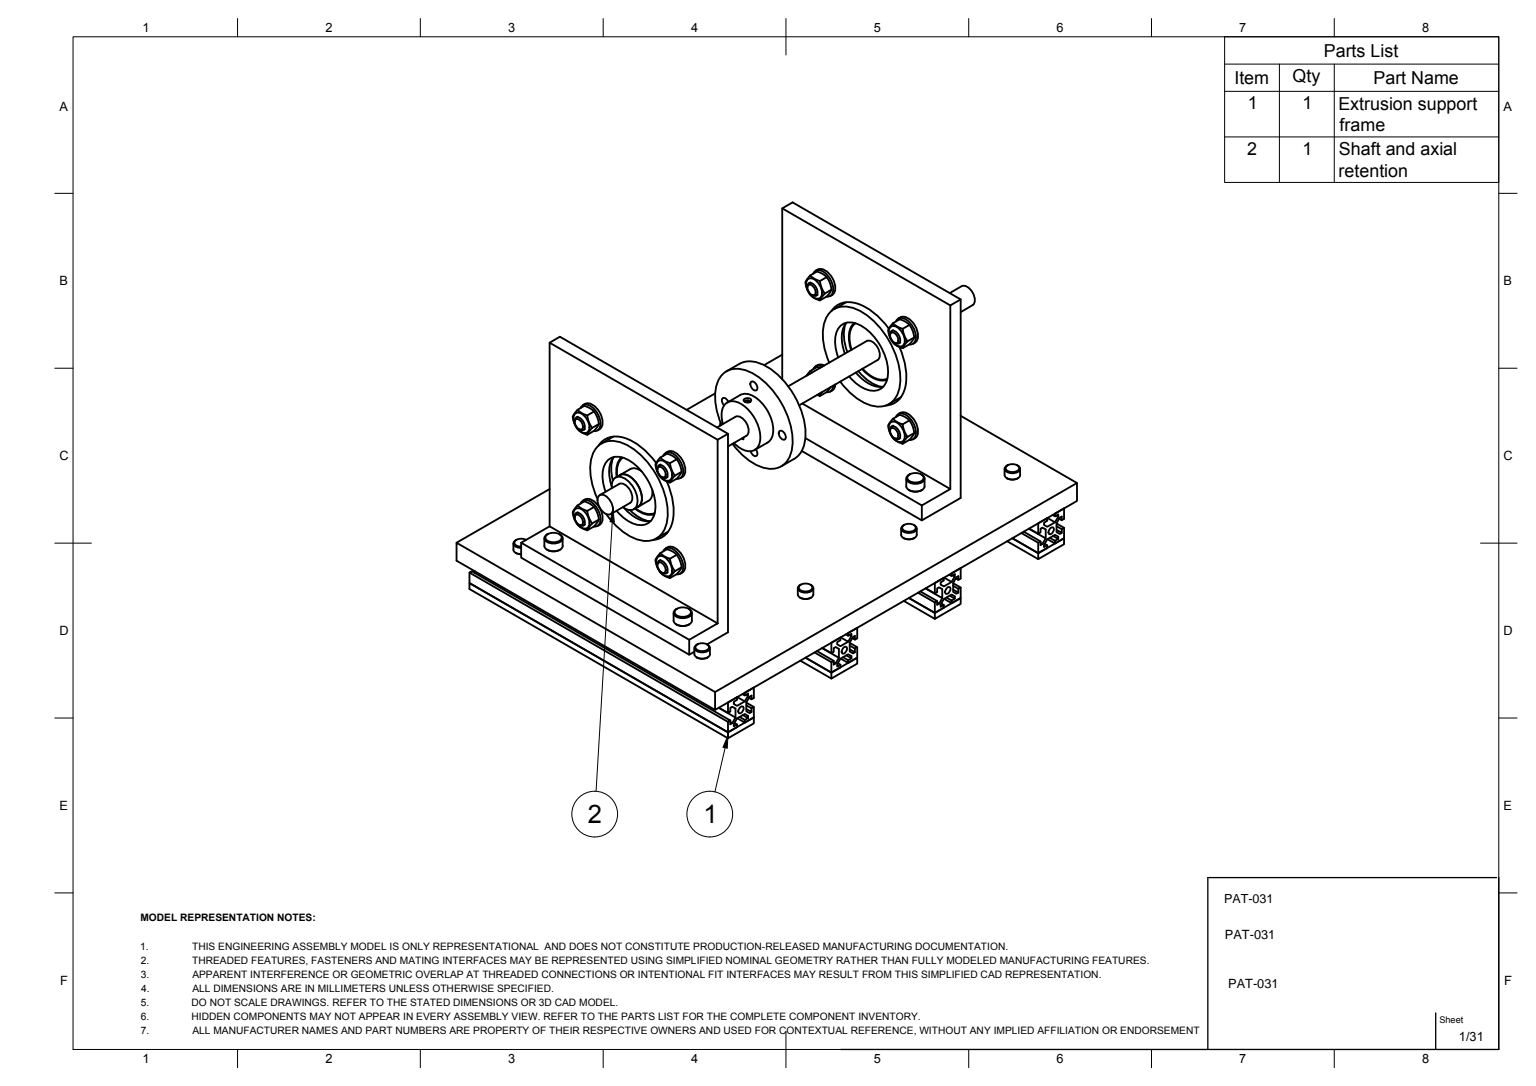
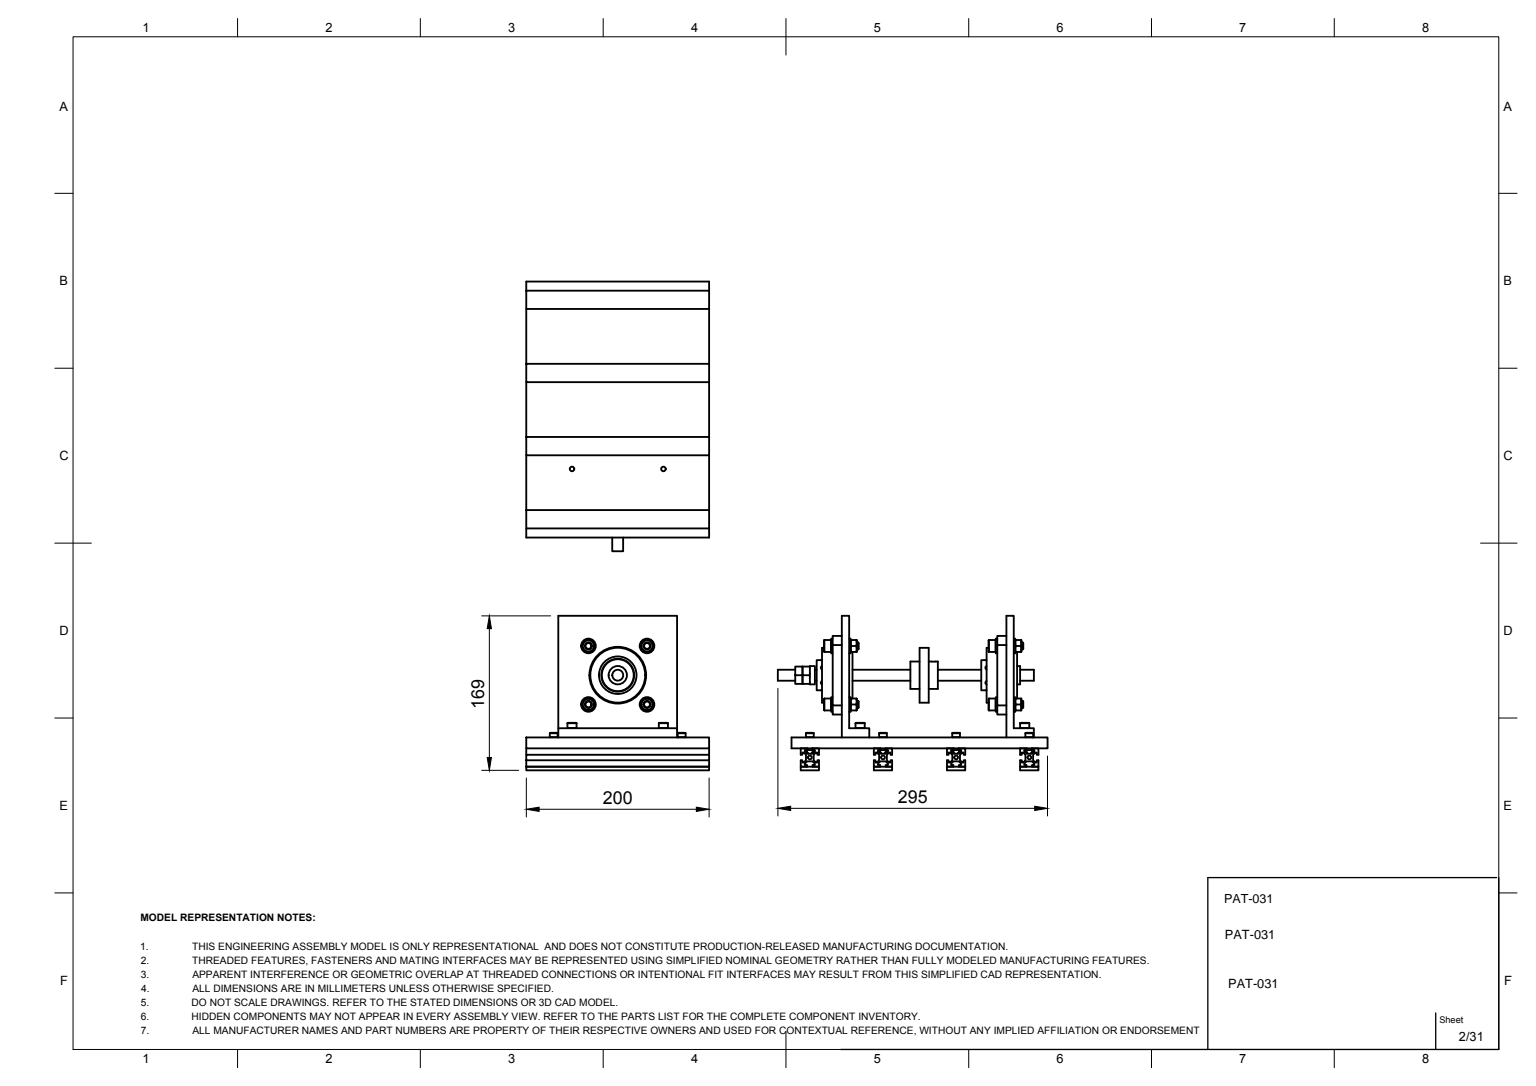
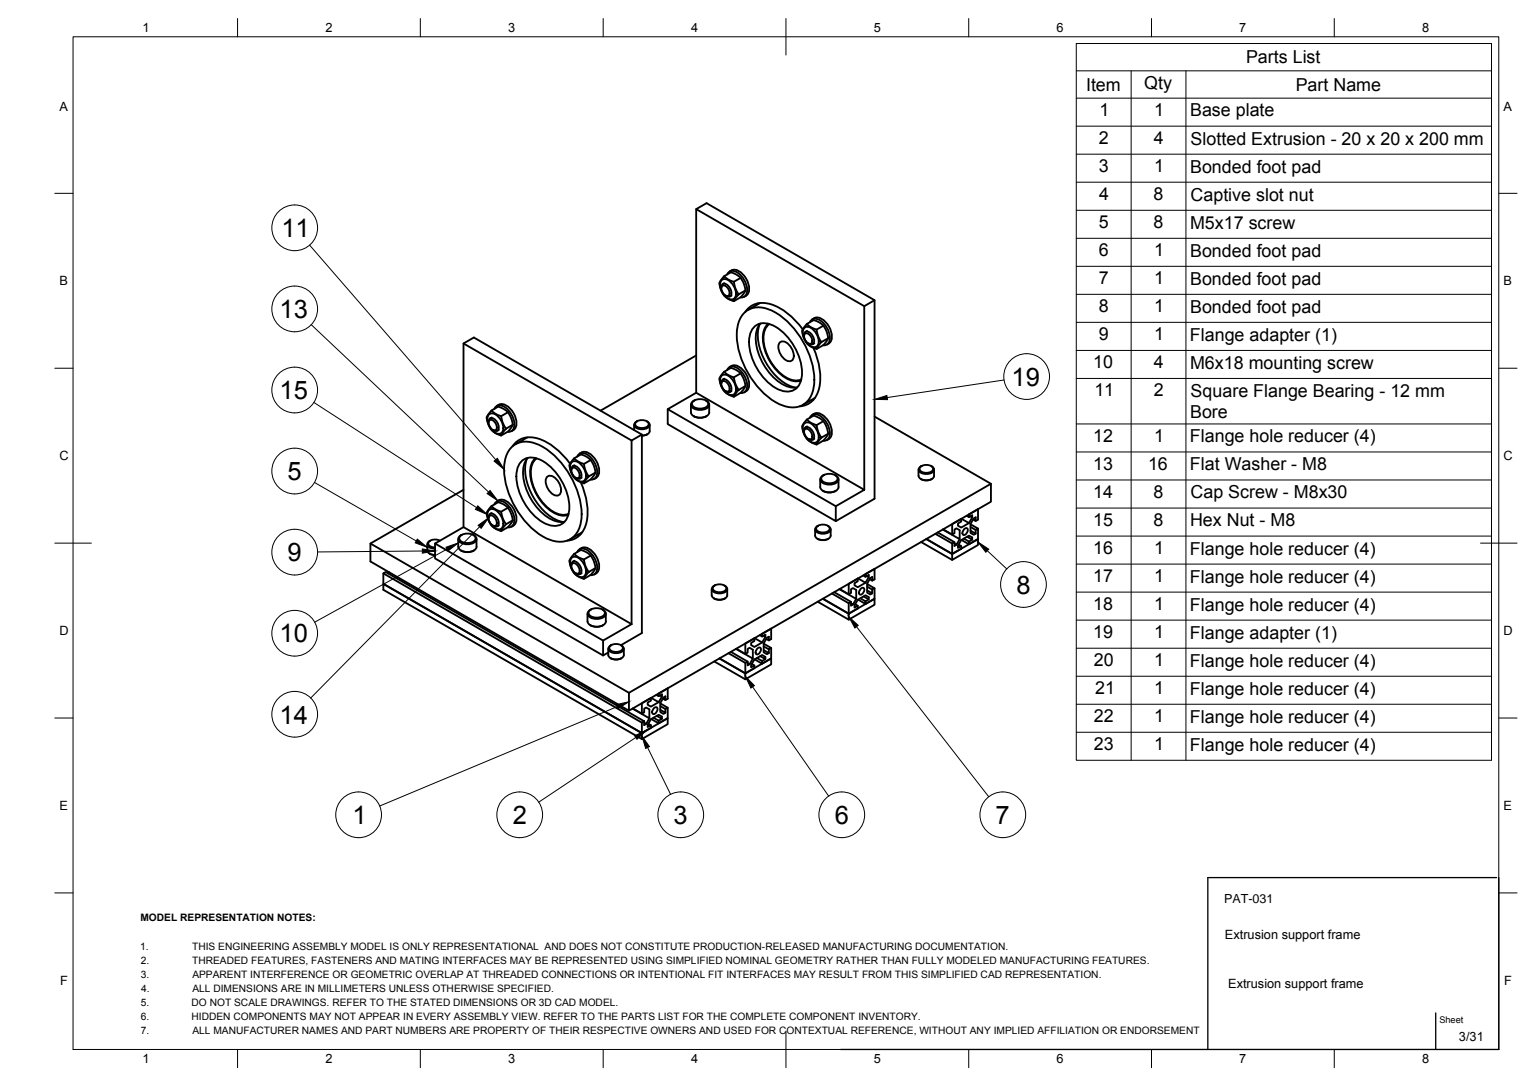
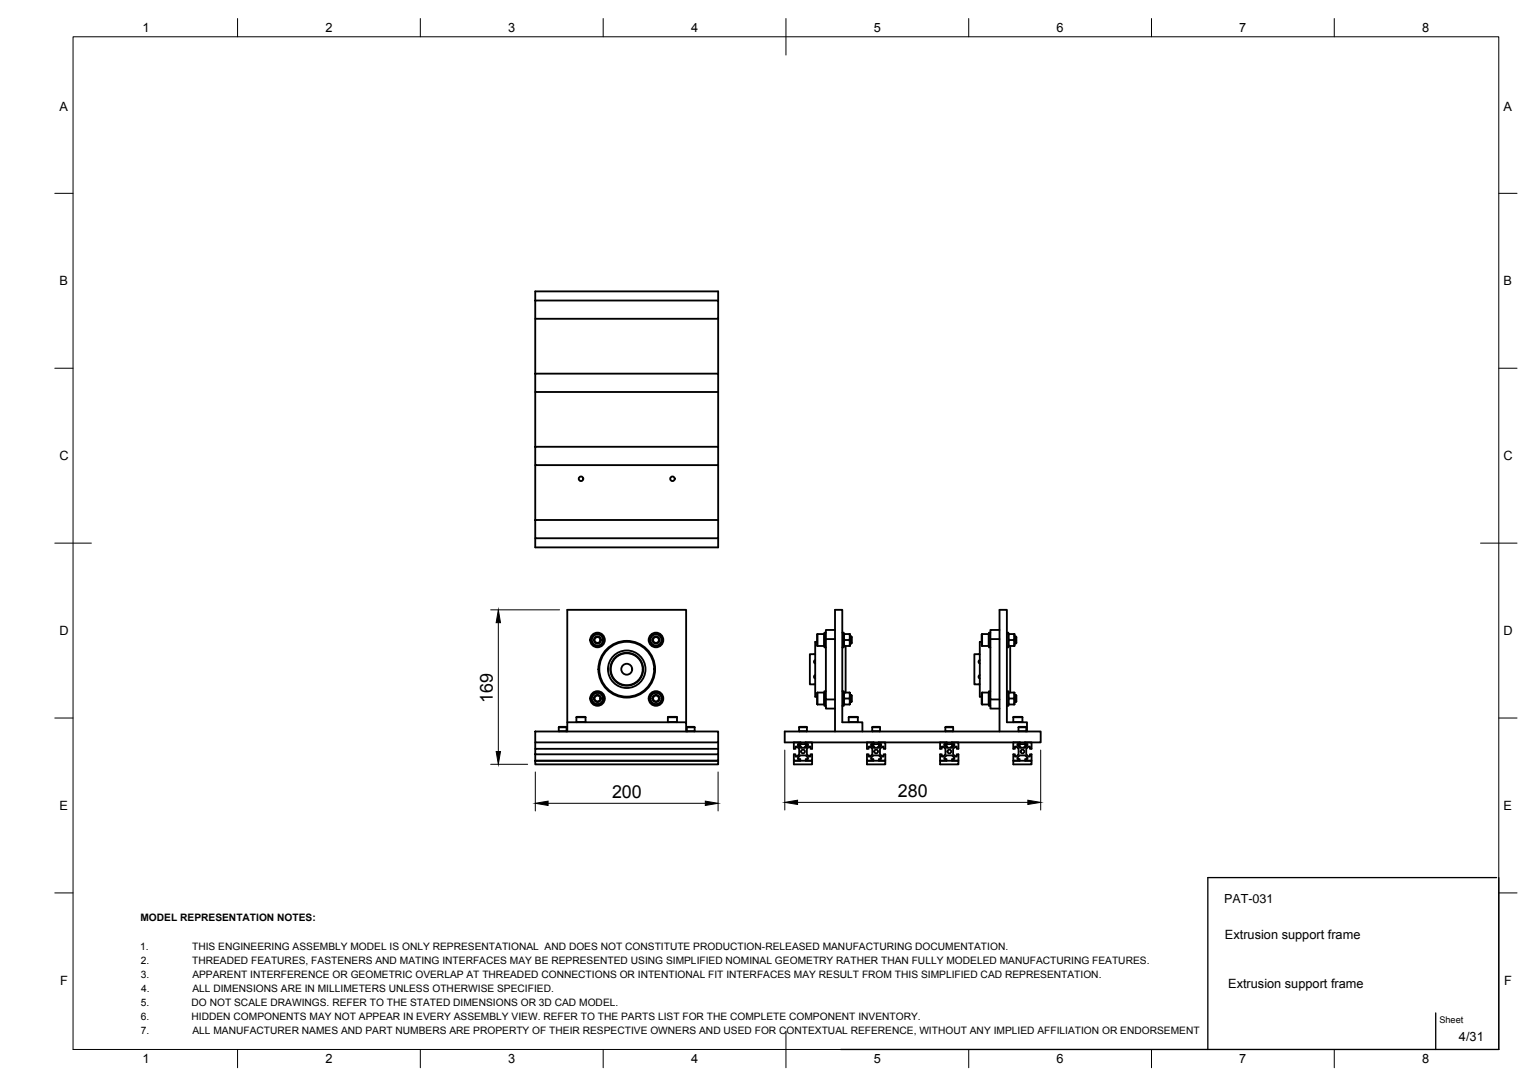
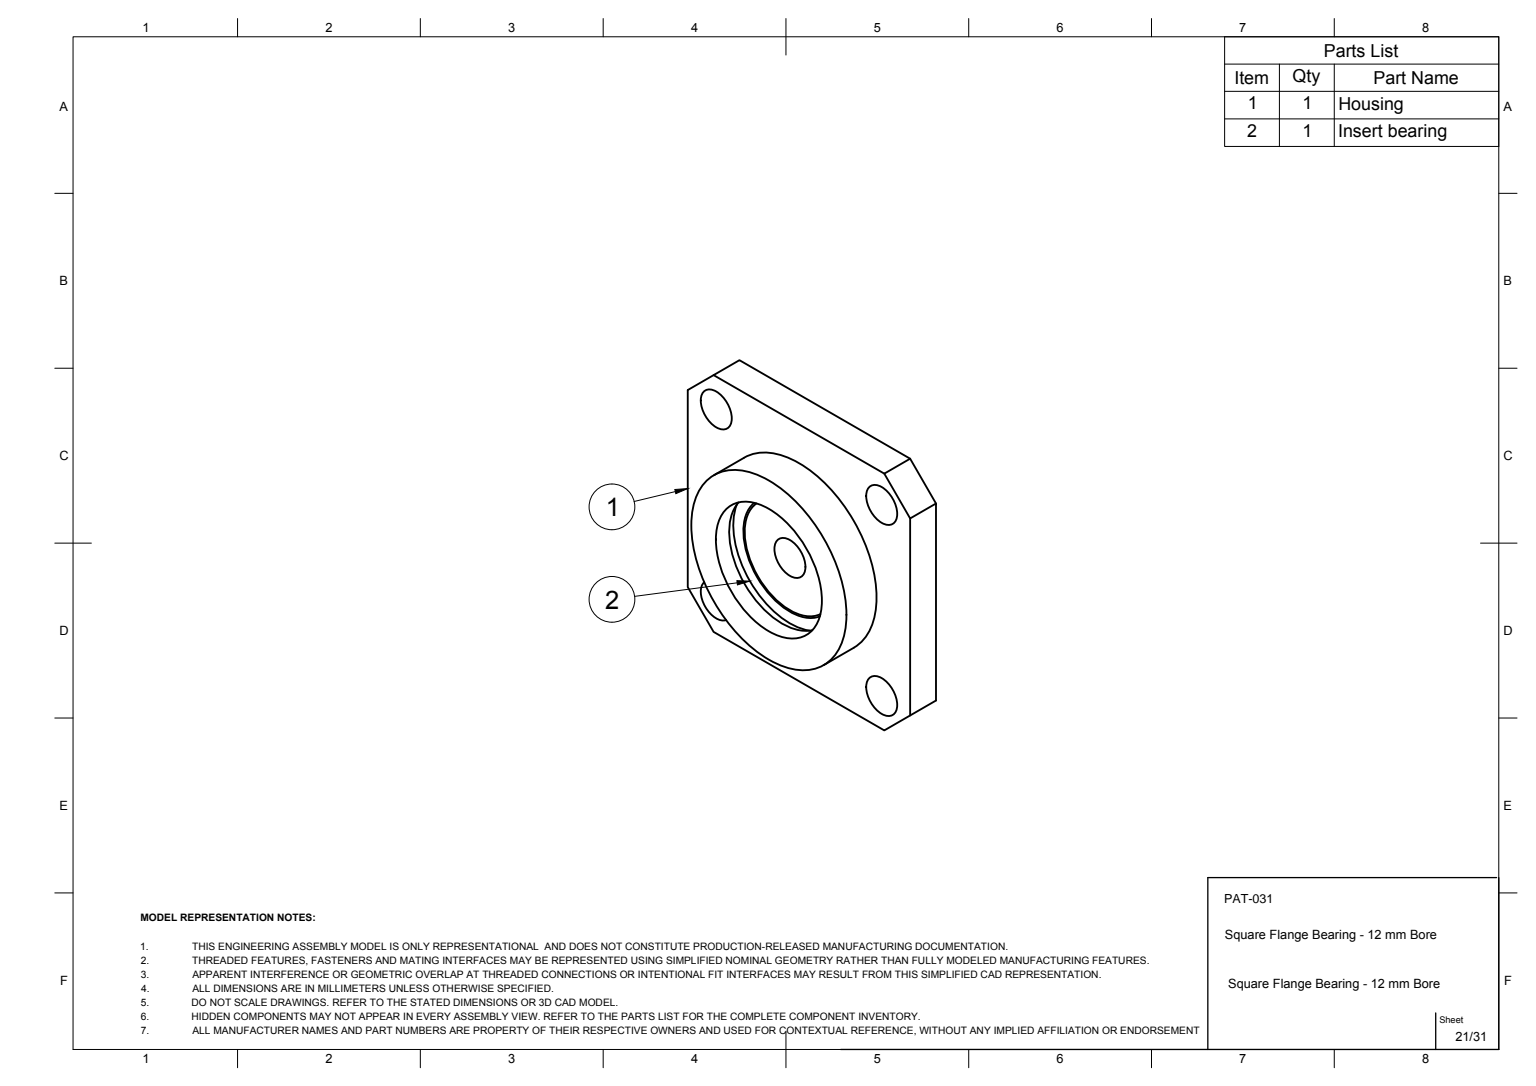
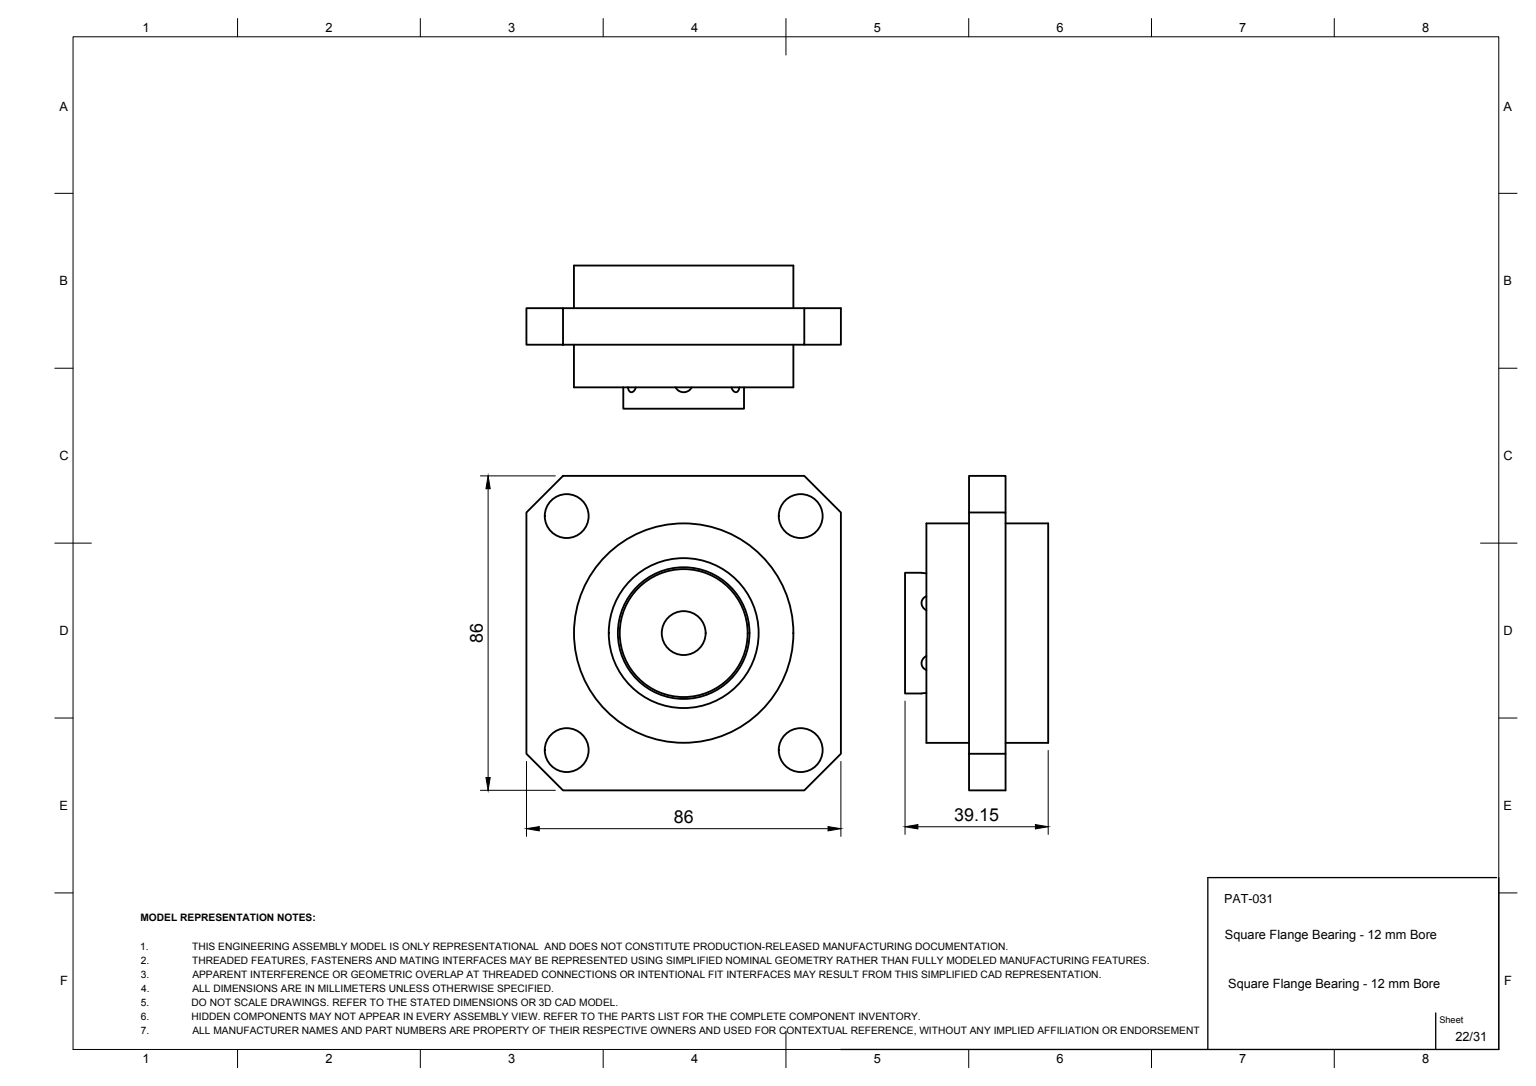
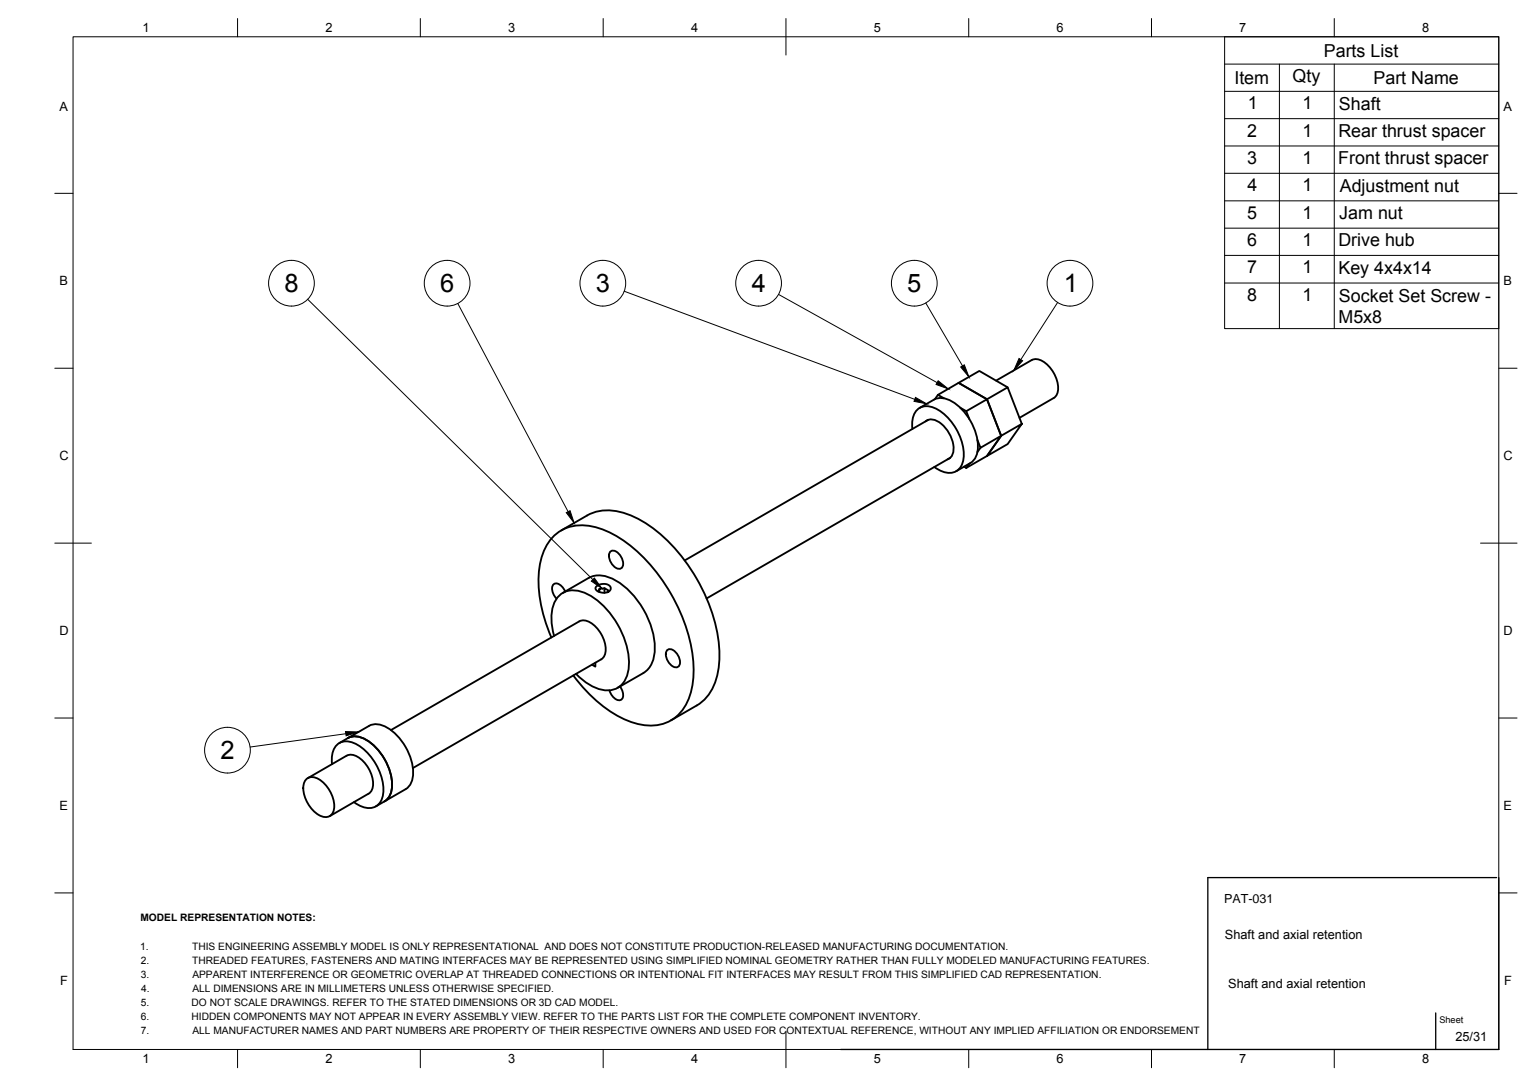
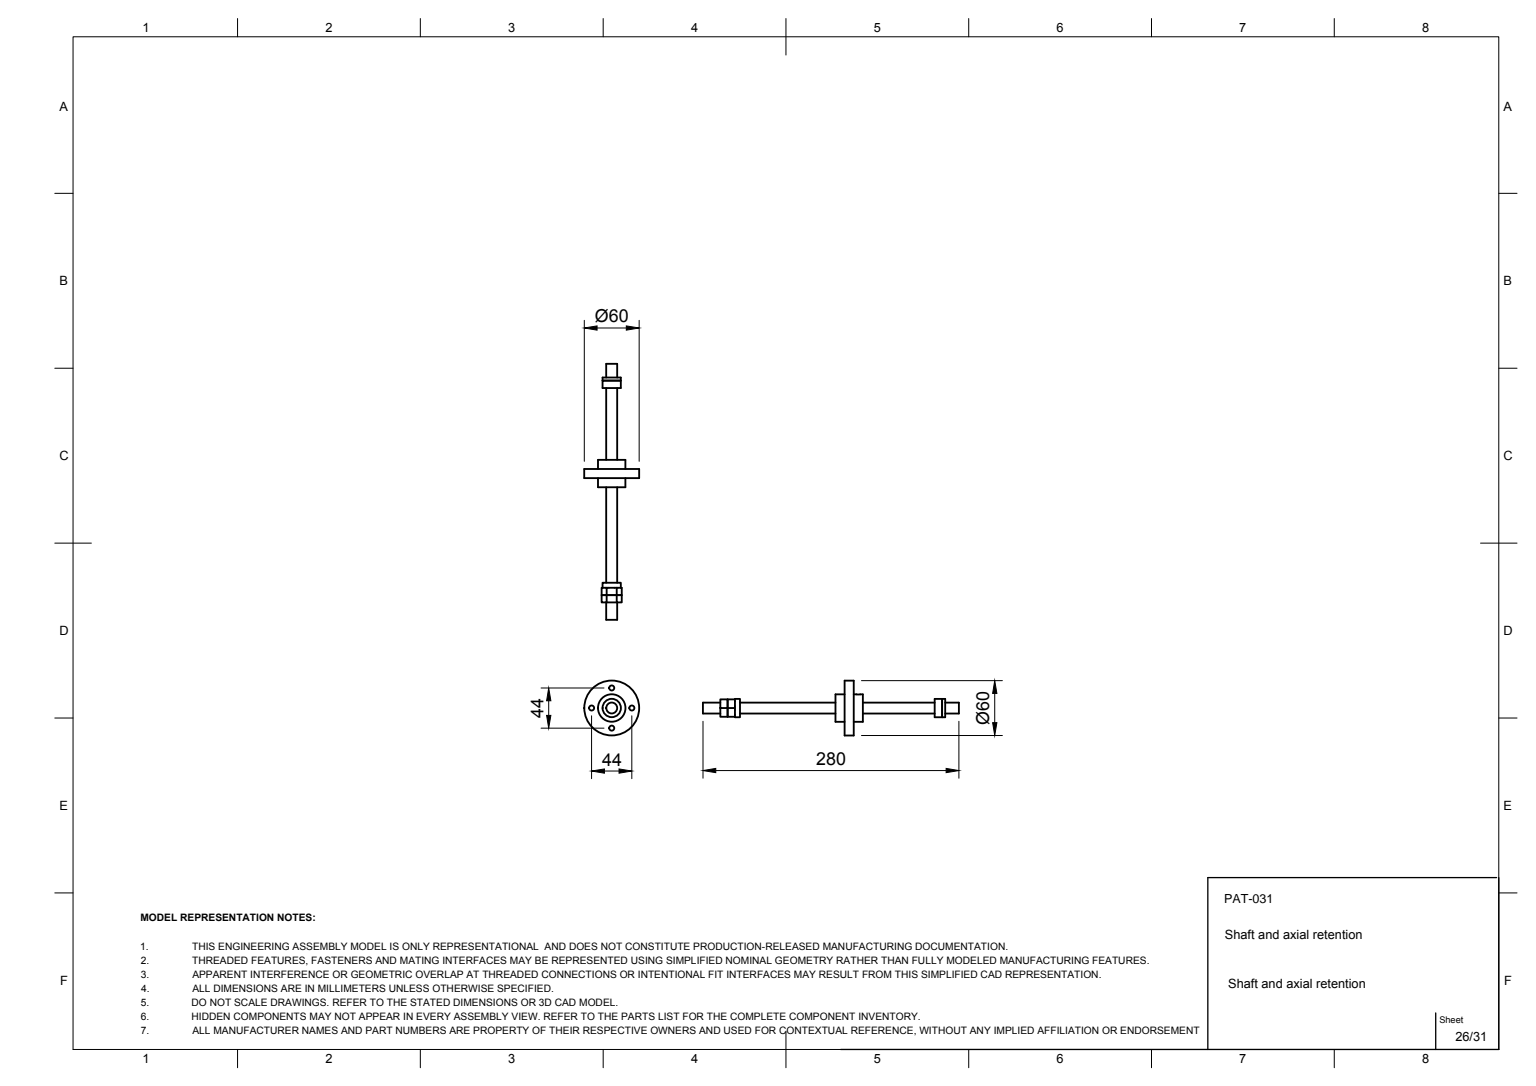
ISO-10303-21;
HEADER;
/* Generated by software containing ST-Developer
 * from STEP Tools, Inc. (www.steptools.com) 
 */

FILE_DESCRIPTION(
/* description */ ('Double-row support with tensioned shaft'),
/* implementation_level */ '2;1');

FILE_NAME(
/* name */ 'PAT-031',
/* time_stamp */ '2026-10-27T10:50:35-07:00',
/* author */ (''),
/* organization */ (''),
/* preprocessor_version */ 'ST-DEVELOPER v20.2',
/* originating_system */ 'Autodesk Translation Framework v15.17.0.0',
/* authorisation */ '');

FILE_SCHEMA (('AUTOMOTIVE_DESIGN { 1 0 10303 214 3 1 1 }'));
ENDSEC;

DATA;
#10=MECHANICAL_DESIGN_GEOMETRIC_PRESENTATION_REPRESENTATION('',(#479,#480,
#481,#482,#483,#484,#485,#486,#487,#488,#489,#490,#491,#492,#493,#494,#495,
#496,#497,#498,#499,#500,#501,#502,#503,#504,#505,#506,#507,#508,#509,#510,
#511),#11559);
#11=(
BOUNDED_CURVE()
B_SPLINE_CURVE(2,(#10913,#10914,#10915),.UNSPECIFIED.,.F.,.F.)
B_SPLINE_CURVE_WITH_KNOTS((3,3),(0.14973948338295,0.97160236658079),
 .UNSPECIFIED.)
CURVE()
GEOMETRIC_REPRESENTATION_ITEM()
RATIONAL_B_SPLINE_CURVE((1.07140024848292,1.23714644374248,1.07140024848292))
REPRESENTATION_ITEM('')
);
#12=(
BOUNDED_CURVE()
B_SPLINE_CURVE(2,(#10917,#10918,#10919),.UNSPECIFIED.,.F.,.F.)
B_SPLINE_CURVE_WITH_KNOTS((3,3),(0.14973948338295,0.971602366580789),
 .UNSPECIFIED.)
CURVE()
GEOMETRIC_REPRESENTATION_ITEM()
RATIONAL_B_SPLINE_CURVE((1.07140024848292,1.23714644374248,1.07140024848292))
REPRESENTATION_ITEM('')
);
#13=(
BOUNDED_CURVE()
B_SPLINE_CURVE(2,(#10924,#10925,#10926),.UNSPECIFIED.,.F.,.F.)
B_SPLINE_CURVE_WITH_KNOTS((3,3),(0.14973948338295,0.97160236658079),
 .UNSPECIFIED.)
CURVE()
GEOMETRIC_REPRESENTATION_ITEM()
RATIONAL_B_SPLINE_CURVE((1.07140024848292,1.23714644374248,1.07140024848292))
REPRESENTATION_ITEM('')
);
#14=(
BOUNDED_CURVE()
B_SPLINE_CURVE(2,(#10928,#10929,#10930),.UNSPECIFIED.,.F.,.F.)
B_SPLINE_CURVE_WITH_KNOTS((3,3),(0.14973948338295,0.97160236658079),
 .UNSPECIFIED.)
CURVE()
GEOMETRIC_REPRESENTATION_ITEM()
RATIONAL_B_SPLINE_CURVE((1.07140024848292,1.23714644374248,1.07140024848292))
REPRESENTATION_ITEM('')
);
#15=(
BOUNDED_CURVE()
B_SPLINE_CURVE(2,(#10932,#10933,#10934),.UNSPECIFIED.,.F.,.F.)
B_SPLINE_CURVE_WITH_KNOTS((3,3),(0.14973948338295,0.971602366580789),
 .UNSPECIFIED.)
CURVE()
GEOMETRIC_REPRESENTATION_ITEM()
RATIONAL_B_SPLINE_CURVE((1.07140024848292,1.23714644374248,1.07140024848292))
REPRESENTATION_ITEM('')
);
#16=(
BOUNDED_CURVE()
B_SPLINE_CURVE(2,(#10935,#10936,#10937),.UNSPECIFIED.,.F.,.F.)
B_SPLINE_CURVE_WITH_KNOTS((3,3),(0.14973948338295,0.97160236658079),
 .UNSPECIFIED.)
CURVE()
GEOMETRIC_REPRESENTATION_ITEM()
RATIONAL_B_SPLINE_CURVE((1.07140024848292,1.23714644374248,1.07140024848292))
REPRESENTATION_ITEM('')
);
#17=(
BOUNDED_CURVE()
B_SPLINE_CURVE(2,(#10944,#10945,#10946),.UNSPECIFIED.,.F.,.F.)
B_SPLINE_CURVE_WITH_KNOTS((3,3),(0.14973948338295,0.97160236658079),
 .UNSPECIFIED.)
CURVE()
GEOMETRIC_REPRESENTATION_ITEM()
RATIONAL_B_SPLINE_CURVE((1.07140024848292,1.23714644374248,1.07140024848292))
REPRESENTATION_ITEM('')
);
#18=(
BOUNDED_CURVE()
B_SPLINE_CURVE(2,(#10948,#10949,#10950),.UNSPECIFIED.,.F.,.F.)
B_SPLINE_CURVE_WITH_KNOTS((3,3),(0.14973948338295,0.97160236658079),
 .UNSPECIFIED.)
CURVE()
GEOMETRIC_REPRESENTATION_ITEM()
RATIONAL_B_SPLINE_CURVE((1.07140024848292,1.23714644374248,1.07140024848292))
REPRESENTATION_ITEM('')
);
#19=(
BOUNDED_CURVE()
B_SPLINE_CURVE(2,(#10952,#10953,#10954),.UNSPECIFIED.,.F.,.F.)
B_SPLINE_CURVE_WITH_KNOTS((3,3),(0.14973948338295,0.971602366580789),
 .UNSPECIFIED.)
CURVE()
GEOMETRIC_REPRESENTATION_ITEM()
RATIONAL_B_SPLINE_CURVE((1.07140024848292,1.23714644374248,1.07140024848292))
REPRESENTATION_ITEM('')
);
#20=(
BOUNDED_CURVE()
B_SPLINE_CURVE(2,(#10956,#10957,#10958),.UNSPECIFIED.,.F.,.F.)
B_SPLINE_CURVE_WITH_KNOTS((3,3),(0.14973948338295,0.97160236658079),
 .UNSPECIFIED.)
CURVE()
GEOMETRIC_REPRESENTATION_ITEM()
RATIONAL_B_SPLINE_CURVE((1.07140024848292,1.23714644374248,1.07140024848292))
REPRESENTATION_ITEM('')
);
#21=(
BOUNDED_CURVE()
B_SPLINE_CURVE(2,(#10960,#10961,#10962),.UNSPECIFIED.,.F.,.F.)
B_SPLINE_CURVE_WITH_KNOTS((3,3),(0.14973948338295,0.97160236658079),
 .UNSPECIFIED.)
CURVE()
GEOMETRIC_REPRESENTATION_ITEM()
RATIONAL_B_SPLINE_CURVE((1.07140024848292,1.23714644374248,1.07140024848292))
REPRESENTATION_ITEM('')
);
#22=(
BOUNDED_CURVE()
B_SPLINE_CURVE(2,(#10963,#10964,#10965),.UNSPECIFIED.,.F.,.F.)
B_SPLINE_CURVE_WITH_KNOTS((3,3),(0.14973948338295,0.971602366580789),
 .UNSPECIFIED.)
CURVE()
GEOMETRIC_REPRESENTATION_ITEM()
RATIONAL_B_SPLINE_CURVE((1.07140024848292,1.23714644374248,1.07140024848292))
REPRESENTATION_ITEM('')
);
#23=ITEM_DEFINED_TRANSFORMATION($,$,#7038,#7105);
#24=ITEM_DEFINED_TRANSFORMATION($,$,#7077,#7106);
#25=ITEM_DEFINED_TRANSFORMATION($,$,#6715,#7158);
#26=ITEM_DEFINED_TRANSFORMATION($,$,#6758,#7159);
#27=ITEM_DEFINED_TRANSFORMATION($,$,#6765,#7160);
#28=ITEM_DEFINED_TRANSFORMATION($,$,#6772,#7161);
#29=ITEM_DEFINED_TRANSFORMATION($,$,#6779,#7162);
#30=ITEM_DEFINED_TRANSFORMATION($,$,#6786,#7163);
#31=ITEM_DEFINED_TRANSFORMATION($,$,#6816,#7164);
#32=ITEM_DEFINED_TRANSFORMATION($,$,#6825,#7165);
#33=ITEM_DEFINED_TRANSFORMATION($,$,#6834,#7166);
#34=ITEM_DEFINED_TRANSFORMATION($,$,#6843,#7167);
#35=ITEM_DEFINED_TRANSFORMATION($,$,#6852,#7168);
#36=ITEM_DEFINED_TRANSFORMATION($,$,#6882,#7169);
#37=ITEM_DEFINED_TRANSFORMATION($,$,#6891,#7170);
#38=ITEM_DEFINED_TRANSFORMATION($,$,#6900,#7171);
#39=ITEM_DEFINED_TRANSFORMATION($,$,#6909,#7172);
#40=ITEM_DEFINED_TRANSFORMATION($,$,#6918,#7173);
#41=ITEM_DEFINED_TRANSFORMATION($,$,#6968,#7174);
#42=ITEM_DEFINED_TRANSFORMATION($,$,#6989,#7175);
#43=ITEM_DEFINED_TRANSFORMATION($,$,#6968,#7176);
#44=ITEM_DEFINED_TRANSFORMATION($,$,#6989,#7177);
#45=ITEM_DEFINED_TRANSFORMATION($,$,#6918,#7178);
#46=ITEM_DEFINED_TRANSFORMATION($,$,#6968,#7179);
#47=ITEM_DEFINED_TRANSFORMATION($,$,#6989,#7180);
#48=ITEM_DEFINED_TRANSFORMATION($,$,#6968,#7181);
#49=ITEM_DEFINED_TRANSFORMATION($,$,#6989,#7182);
#50=ITEM_DEFINED_TRANSFORMATION($,$,#6918,#7183);
#51=ITEM_DEFINED_TRANSFORMATION($,$,#6968,#7184);
#52=ITEM_DEFINED_TRANSFORMATION($,$,#6989,#7185);
#53=ITEM_DEFINED_TRANSFORMATION($,$,#6968,#7186);
#54=ITEM_DEFINED_TRANSFORMATION($,$,#6989,#7187);
#55=ITEM_DEFINED_TRANSFORMATION($,$,#6918,#7188);
#56=ITEM_DEFINED_TRANSFORMATION($,$,#6968,#7189);
#57=ITEM_DEFINED_TRANSFORMATION($,$,#6989,#7190);
#58=ITEM_DEFINED_TRANSFORMATION($,$,#6968,#7191);
#59=ITEM_DEFINED_TRANSFORMATION($,$,#6989,#7192);
#60=ITEM_DEFINED_TRANSFORMATION($,$,#7013,#7193);
#61=ITEM_DEFINED_TRANSFORMATION($,$,#7013,#7194);
#62=ITEM_DEFINED_TRANSFORMATION($,$,#7037,#7195);
#63=ITEM_DEFINED_TRANSFORMATION($,$,#7133,#7196);
#64=ITEM_DEFINED_TRANSFORMATION($,$,#7107,#7197);
#65=ITEM_DEFINED_TRANSFORMATION($,$,#7133,#7198);
#66=ITEM_DEFINED_TRANSFORMATION($,$,#7142,#7199);
#67=ITEM_DEFINED_TRANSFORMATION($,$,#7133,#7200);
#68=ITEM_DEFINED_TRANSFORMATION($,$,#7107,#7201);
#69=ITEM_DEFINED_TRANSFORMATION($,$,#7133,#7202);
#70=ITEM_DEFINED_TRANSFORMATION($,$,#7142,#7203);
#71=ITEM_DEFINED_TRANSFORMATION($,$,#7133,#7204);
#72=ITEM_DEFINED_TRANSFORMATION($,$,#7107,#7205);
#73=ITEM_DEFINED_TRANSFORMATION($,$,#7133,#7206);
#74=ITEM_DEFINED_TRANSFORMATION($,$,#7142,#7207);
#75=ITEM_DEFINED_TRANSFORMATION($,$,#7133,#7208);
#76=ITEM_DEFINED_TRANSFORMATION($,$,#7107,#7209);
#77=ITEM_DEFINED_TRANSFORMATION($,$,#7133,#7210);
#78=ITEM_DEFINED_TRANSFORMATION($,$,#7142,#7211);
#79=ITEM_DEFINED_TRANSFORMATION($,$,#7013,#7212);
#80=ITEM_DEFINED_TRANSFORMATION($,$,#7013,#7213);
#81=ITEM_DEFINED_TRANSFORMATION($,$,#7037,#7214);
#82=ITEM_DEFINED_TRANSFORMATION($,$,#7133,#7215);
#83=ITEM_DEFINED_TRANSFORMATION($,$,#7107,#7216);
#84=ITEM_DEFINED_TRANSFORMATION($,$,#7133,#7217);
#85=ITEM_DEFINED_TRANSFORMATION($,$,#7142,#7218);
#86=ITEM_DEFINED_TRANSFORMATION($,$,#7133,#7219);
#87=ITEM_DEFINED_TRANSFORMATION($,$,#7107,#7220);
#88=ITEM_DEFINED_TRANSFORMATION($,$,#7133,#7221);
#89=ITEM_DEFINED_TRANSFORMATION($,$,#7142,#7222);
#90=ITEM_DEFINED_TRANSFORMATION($,$,#7133,#7223);
#91=ITEM_DEFINED_TRANSFORMATION($,$,#7107,#7224);
#92=ITEM_DEFINED_TRANSFORMATION($,$,#7133,#7225);
#93=ITEM_DEFINED_TRANSFORMATION($,$,#7142,#7226);
#94=ITEM_DEFINED_TRANSFORMATION($,$,#7133,#7227);
#95=ITEM_DEFINED_TRANSFORMATION($,$,#7107,#7228);
#96=ITEM_DEFINED_TRANSFORMATION($,$,#7133,#7229);
#97=ITEM_DEFINED_TRANSFORMATION($,$,#7142,#7230);
#98=ITEM_DEFINED_TRANSFORMATION($,$,#7232,#7361);
#99=ITEM_DEFINED_TRANSFORMATION($,$,#7253,#7362);
#100=ITEM_DEFINED_TRANSFORMATION($,$,#7262,#7363);
#101=ITEM_DEFINED_TRANSFORMATION($,$,#7271,#7364);
#102=ITEM_DEFINED_TRANSFORMATION($,$,#7283,#7365);
#103=ITEM_DEFINED_TRANSFORMATION($,$,#7295,#7366);
#104=ITEM_DEFINED_TRANSFORMATION($,$,#7333,#7367);
#105=ITEM_DEFINED_TRANSFORMATION($,$,#7344,#7368);
#106=ITEM_DEFINED_TRANSFORMATION($,$,#6714,#7369);
#107=ITEM_DEFINED_TRANSFORMATION($,$,#7231,#7370);
#108=(
REPRESENTATION_RELATIONSHIP($,$,#11743,#11742)
REPRESENTATION_RELATIONSHIP_WITH_TRANSFORMATION(#23)
SHAPE_REPRESENTATION_RELATIONSHIP()
);
#109=(
REPRESENTATION_RELATIONSHIP($,$,#11744,#11742)
REPRESENTATION_RELATIONSHIP_WITH_TRANSFORMATION(#24)
SHAPE_REPRESENTATION_RELATIONSHIP()
);
#110=(
REPRESENTATION_RELATIONSHIP($,$,#11723,#11722)
REPRESENTATION_RELATIONSHIP_WITH_TRANSFORMATION(#25)
SHAPE_REPRESENTATION_RELATIONSHIP()
);
#111=(
REPRESENTATION_RELATIONSHIP($,$,#11724,#11722)
REPRESENTATION_RELATIONSHIP_WITH_TRANSFORMATION(#26)
SHAPE_REPRESENTATION_RELATIONSHIP()
);
#112=(
REPRESENTATION_RELATIONSHIP($,$,#11725,#11722)
REPRESENTATION_RELATIONSHIP_WITH_TRANSFORMATION(#27)
SHAPE_REPRESENTATION_RELATIONSHIP()
);
#113=(
REPRESENTATION_RELATIONSHIP($,$,#11726,#11722)
REPRESENTATION_RELATIONSHIP_WITH_TRANSFORMATION(#28)
SHAPE_REPRESENTATION_RELATIONSHIP()
);
#114=(
REPRESENTATION_RELATIONSHIP($,$,#11727,#11722)
REPRESENTATION_RELATIONSHIP_WITH_TRANSFORMATION(#29)
SHAPE_REPRESENTATION_RELATIONSHIP()
);
#115=(
REPRESENTATION_RELATIONSHIP($,$,#11728,#11722)
REPRESENTATION_RELATIONSHIP_WITH_TRANSFORMATION(#30)
SHAPE_REPRESENTATION_RELATIONSHIP()
);
#116=(
REPRESENTATION_RELATIONSHIP($,$,#11729,#11722)
REPRESENTATION_RELATIONSHIP_WITH_TRANSFORMATION(#31)
SHAPE_REPRESENTATION_RELATIONSHIP()
);
#117=(
REPRESENTATION_RELATIONSHIP($,$,#11730,#11722)
REPRESENTATION_RELATIONSHIP_WITH_TRANSFORMATION(#32)
SHAPE_REPRESENTATION_RELATIONSHIP()
);
#118=(
REPRESENTATION_RELATIONSHIP($,$,#11731,#11722)
REPRESENTATION_RELATIONSHIP_WITH_TRANSFORMATION(#33)
SHAPE_REPRESENTATION_RELATIONSHIP()
);
#119=(
REPRESENTATION_RELATIONSHIP($,$,#11732,#11722)
REPRESENTATION_RELATIONSHIP_WITH_TRANSFORMATION(#34)
SHAPE_REPRESENTATION_RELATIONSHIP()
);
#120=(
REPRESENTATION_RELATIONSHIP($,$,#11733,#11722)
REPRESENTATION_RELATIONSHIP_WITH_TRANSFORMATION(#35)
SHAPE_REPRESENTATION_RELATIONSHIP()
);
#121=(
REPRESENTATION_RELATIONSHIP($,$,#11734,#11722)
REPRESENTATION_RELATIONSHIP_WITH_TRANSFORMATION(#36)
SHAPE_REPRESENTATION_RELATIONSHIP()
);
#122=(
REPRESENTATION_RELATIONSHIP($,$,#11735,#11722)
REPRESENTATION_RELATIONSHIP_WITH_TRANSFORMATION(#37)
SHAPE_REPRESENTATION_RELATIONSHIP()
);
#123=(
REPRESENTATION_RELATIONSHIP($,$,#11736,#11722)
REPRESENTATION_RELATIONSHIP_WITH_TRANSFORMATION(#38)
SHAPE_REPRESENTATION_RELATIONSHIP()
);
#124=(
REPRESENTATION_RELATIONSHIP($,$,#11737,#11722)
REPRESENTATION_RELATIONSHIP_WITH_TRANSFORMATION(#39)
SHAPE_REPRESENTATION_RELATIONSHIP()
);
#125=(
REPRESENTATION_RELATIONSHIP($,$,#11738,#11722)
REPRESENTATION_RELATIONSHIP_WITH_TRANSFORMATION(#40)
SHAPE_REPRESENTATION_RELATIONSHIP()
);
#126=(
REPRESENTATION_RELATIONSHIP($,$,#11739,#11722)
REPRESENTATION_RELATIONSHIP_WITH_TRANSFORMATION(#41)
SHAPE_REPRESENTATION_RELATIONSHIP()
);
#127=(
REPRESENTATION_RELATIONSHIP($,$,#11740,#11722)
REPRESENTATION_RELATIONSHIP_WITH_TRANSFORMATION(#42)
SHAPE_REPRESENTATION_RELATIONSHIP()
);
#128=(
REPRESENTATION_RELATIONSHIP($,$,#11739,#11722)
REPRESENTATION_RELATIONSHIP_WITH_TRANSFORMATION(#43)
SHAPE_REPRESENTATION_RELATIONSHIP()
);
#129=(
REPRESENTATION_RELATIONSHIP($,$,#11740,#11722)
REPRESENTATION_RELATIONSHIP_WITH_TRANSFORMATION(#44)
SHAPE_REPRESENTATION_RELATIONSHIP()
);
#130=(
REPRESENTATION_RELATIONSHIP($,$,#11738,#11722)
REPRESENTATION_RELATIONSHIP_WITH_TRANSFORMATION(#45)
SHAPE_REPRESENTATION_RELATIONSHIP()
);
#131=(
REPRESENTATION_RELATIONSHIP($,$,#11739,#11722)
REPRESENTATION_RELATIONSHIP_WITH_TRANSFORMATION(#46)
SHAPE_REPRESENTATION_RELATIONSHIP()
);
#132=(
REPRESENTATION_RELATIONSHIP($,$,#11740,#11722)
REPRESENTATION_RELATIONSHIP_WITH_TRANSFORMATION(#47)
SHAPE_REPRESENTATION_RELATIONSHIP()
);
#133=(
REPRESENTATION_RELATIONSHIP($,$,#11739,#11722)
REPRESENTATION_RELATIONSHIP_WITH_TRANSFORMATION(#48)
SHAPE_REPRESENTATION_RELATIONSHIP()
);
#134=(
REPRESENTATION_RELATIONSHIP($,$,#11740,#11722)
REPRESENTATION_RELATIONSHIP_WITH_TRANSFORMATION(#49)
SHAPE_REPRESENTATION_RELATIONSHIP()
);
#135=(
REPRESENTATION_RELATIONSHIP($,$,#11738,#11722)
REPRESENTATION_RELATIONSHIP_WITH_TRANSFORMATION(#50)
SHAPE_REPRESENTATION_RELATIONSHIP()
);
#136=(
REPRESENTATION_RELATIONSHIP($,$,#11739,#11722)
REPRESENTATION_RELATIONSHIP_WITH_TRANSFORMATION(#51)
SHAPE_REPRESENTATION_RELATIONSHIP()
);
#137=(
REPRESENTATION_RELATIONSHIP($,$,#11740,#11722)
REPRESENTATION_RELATIONSHIP_WITH_TRANSFORMATION(#52)
SHAPE_REPRESENTATION_RELATIONSHIP()
);
#138=(
REPRESENTATION_RELATIONSHIP($,$,#11739,#11722)
REPRESENTATION_RELATIONSHIP_WITH_TRANSFORMATION(#53)
SHAPE_REPRESENTATION_RELATIONSHIP()
);
#139=(
REPRESENTATION_RELATIONSHIP($,$,#11740,#11722)
REPRESENTATION_RELATIONSHIP_WITH_TRANSFORMATION(#54)
SHAPE_REPRESENTATION_RELATIONSHIP()
);
#140=(
REPRESENTATION_RELATIONSHIP($,$,#11738,#11722)
REPRESENTATION_RELATIONSHIP_WITH_TRANSFORMATION(#55)
SHAPE_REPRESENTATION_RELATIONSHIP()
);
#141=(
REPRESENTATION_RELATIONSHIP($,$,#11739,#11722)
REPRESENTATION_RELATIONSHIP_WITH_TRANSFORMATION(#56)
SHAPE_REPRESENTATION_RELATIONSHIP()
);
#142=(
REPRESENTATION_RELATIONSHIP($,$,#11740,#11722)
REPRESENTATION_RELATIONSHIP_WITH_TRANSFORMATION(#57)
SHAPE_REPRESENTATION_RELATIONSHIP()
);
#143=(
REPRESENTATION_RELATIONSHIP($,$,#11739,#11722)
REPRESENTATION_RELATIONSHIP_WITH_TRANSFORMATION(#58)
SHAPE_REPRESENTATION_RELATIONSHIP()
);
#144=(
REPRESENTATION_RELATIONSHIP($,$,#11740,#11722)
REPRESENTATION_RELATIONSHIP_WITH_TRANSFORMATION(#59)
SHAPE_REPRESENTATION_RELATIONSHIP()
);
#145=(
REPRESENTATION_RELATIONSHIP($,$,#11741,#11722)
REPRESENTATION_RELATIONSHIP_WITH_TRANSFORMATION(#60)
SHAPE_REPRESENTATION_RELATIONSHIP()
);
#146=(
REPRESENTATION_RELATIONSHIP($,$,#11741,#11722)
REPRESENTATION_RELATIONSHIP_WITH_TRANSFORMATION(#61)
SHAPE_REPRESENTATION_RELATIONSHIP()
);
#147=(
REPRESENTATION_RELATIONSHIP($,$,#11742,#11722)
REPRESENTATION_RELATIONSHIP_WITH_TRANSFORMATION(#62)
SHAPE_REPRESENTATION_RELATIONSHIP()
);
#148=(
REPRESENTATION_RELATIONSHIP($,$,#11746,#11722)
REPRESENTATION_RELATIONSHIP_WITH_TRANSFORMATION(#63)
SHAPE_REPRESENTATION_RELATIONSHIP()
);
#149=(
REPRESENTATION_RELATIONSHIP($,$,#11745,#11722)
REPRESENTATION_RELATIONSHIP_WITH_TRANSFORMATION(#64)
SHAPE_REPRESENTATION_RELATIONSHIP()
);
#150=(
REPRESENTATION_RELATIONSHIP($,$,#11746,#11722)
REPRESENTATION_RELATIONSHIP_WITH_TRANSFORMATION(#65)
SHAPE_REPRESENTATION_RELATIONSHIP()
);
#151=(
REPRESENTATION_RELATIONSHIP($,$,#11747,#11722)
REPRESENTATION_RELATIONSHIP_WITH_TRANSFORMATION(#66)
SHAPE_REPRESENTATION_RELATIONSHIP()
);
#152=(
REPRESENTATION_RELATIONSHIP($,$,#11746,#11722)
REPRESENTATION_RELATIONSHIP_WITH_TRANSFORMATION(#67)
SHAPE_REPRESENTATION_RELATIONSHIP()
);
#153=(
REPRESENTATION_RELATIONSHIP($,$,#11745,#11722)
REPRESENTATION_RELATIONSHIP_WITH_TRANSFORMATION(#68)
SHAPE_REPRESENTATION_RELATIONSHIP()
);
#154=(
REPRESENTATION_RELATIONSHIP($,$,#11746,#11722)
REPRESENTATION_RELATIONSHIP_WITH_TRANSFORMATION(#69)
SHAPE_REPRESENTATION_RELATIONSHIP()
);
#155=(
REPRESENTATION_RELATIONSHIP($,$,#11747,#11722)
REPRESENTATION_RELATIONSHIP_WITH_TRANSFORMATION(#70)
SHAPE_REPRESENTATION_RELATIONSHIP()
);
#156=(
REPRESENTATION_RELATIONSHIP($,$,#11746,#11722)
REPRESENTATION_RELATIONSHIP_WITH_TRANSFORMATION(#71)
SHAPE_REPRESENTATION_RELATIONSHIP()
);
#157=(
REPRESENTATION_RELATIONSHIP($,$,#11745,#11722)
REPRESENTATION_RELATIONSHIP_WITH_TRANSFORMATION(#72)
SHAPE_REPRESENTATION_RELATIONSHIP()
);
#158=(
REPRESENTATION_RELATIONSHIP($,$,#11746,#11722)
REPRESENTATION_RELATIONSHIP_WITH_TRANSFORMATION(#73)
SHAPE_REPRESENTATION_RELATIONSHIP()
);
#159=(
REPRESENTATION_RELATIONSHIP($,$,#11747,#11722)
REPRESENTATION_RELATIONSHIP_WITH_TRANSFORMATION(#74)
SHAPE_REPRESENTATION_RELATIONSHIP()
);
#160=(
REPRESENTATION_RELATIONSHIP($,$,#11746,#11722)
REPRESENTATION_RELATIONSHIP_WITH_TRANSFORMATION(#75)
SHAPE_REPRESENTATION_RELATIONSHIP()
);
#161=(
REPRESENTATION_RELATIONSHIP($,$,#11745,#11722)
REPRESENTATION_RELATIONSHIP_WITH_TRANSFORMATION(#76)
SHAPE_REPRESENTATION_RELATIONSHIP()
);
#162=(
REPRESENTATION_RELATIONSHIP($,$,#11746,#11722)
REPRESENTATION_RELATIONSHIP_WITH_TRANSFORMATION(#77)
SHAPE_REPRESENTATION_RELATIONSHIP()
);
#163=(
REPRESENTATION_RELATIONSHIP($,$,#11747,#11722)
REPRESENTATION_RELATIONSHIP_WITH_TRANSFORMATION(#78)
SHAPE_REPRESENTATION_RELATIONSHIP()
);
#164=(
REPRESENTATION_RELATIONSHIP($,$,#11741,#11722)
REPRESENTATION_RELATIONSHIP_WITH_TRANSFORMATION(#79)
SHAPE_REPRESENTATION_RELATIONSHIP()
);
#165=(
REPRESENTATION_RELATIONSHIP($,$,#11741,#11722)
REPRESENTATION_RELATIONSHIP_WITH_TRANSFORMATION(#80)
SHAPE_REPRESENTATION_RELATIONSHIP()
);
#166=(
REPRESENTATION_RELATIONSHIP($,$,#11742,#11722)
REPRESENTATION_RELATIONSHIP_WITH_TRANSFORMATION(#81)
SHAPE_REPRESENTATION_RELATIONSHIP()
);
#167=(
REPRESENTATION_RELATIONSHIP($,$,#11746,#11722)
REPRESENTATION_RELATIONSHIP_WITH_TRANSFORMATION(#82)
SHAPE_REPRESENTATION_RELATIONSHIP()
);
#168=(
REPRESENTATION_RELATIONSHIP($,$,#11745,#11722)
REPRESENTATION_RELATIONSHIP_WITH_TRANSFORMATION(#83)
SHAPE_REPRESENTATION_RELATIONSHIP()
);
#169=(
REPRESENTATION_RELATIONSHIP($,$,#11746,#11722)
REPRESENTATION_RELATIONSHIP_WITH_TRANSFORMATION(#84)
SHAPE_REPRESENTATION_RELATIONSHIP()
);
#170=(
REPRESENTATION_RELATIONSHIP($,$,#11747,#11722)
REPRESENTATION_RELATIONSHIP_WITH_TRANSFORMATION(#85)
SHAPE_REPRESENTATION_RELATIONSHIP()
);
#171=(
REPRESENTATION_RELATIONSHIP($,$,#11746,#11722)
REPRESENTATION_RELATIONSHIP_WITH_TRANSFORMATION(#86)
SHAPE_REPRESENTATION_RELATIONSHIP()
);
#172=(
REPRESENTATION_RELATIONSHIP($,$,#11745,#11722)
REPRESENTATION_RELATIONSHIP_WITH_TRANSFORMATION(#87)
SHAPE_REPRESENTATION_RELATIONSHIP()
);
#173=(
REPRESENTATION_RELATIONSHIP($,$,#11746,#11722)
REPRESENTATION_RELATIONSHIP_WITH_TRANSFORMATION(#88)
SHAPE_REPRESENTATION_RELATIONSHIP()
);
#174=(
REPRESENTATION_RELATIONSHIP($,$,#11747,#11722)
REPRESENTATION_RELATIONSHIP_WITH_TRANSFORMATION(#89)
SHAPE_REPRESENTATION_RELATIONSHIP()
);
#175=(
REPRESENTATION_RELATIONSHIP($,$,#11746,#11722)
REPRESENTATION_RELATIONSHIP_WITH_TRANSFORMATION(#90)
SHAPE_REPRESENTATION_RELATIONSHIP()
);
#176=(
REPRESENTATION_RELATIONSHIP($,$,#11745,#11722)
REPRESENTATION_RELATIONSHIP_WITH_TRANSFORMATION(#91)
SHAPE_REPRESENTATION_RELATIONSHIP()
);
#177=(
REPRESENTATION_RELATIONSHIP($,$,#11746,#11722)
REPRESENTATION_RELATIONSHIP_WITH_TRANSFORMATION(#92)
SHAPE_REPRESENTATION_RELATIONSHIP()
);
#178=(
REPRESENTATION_RELATIONSHIP($,$,#11747,#11722)
REPRESENTATION_RELATIONSHIP_WITH_TRANSFORMATION(#93)
SHAPE_REPRESENTATION_RELATIONSHIP()
);
#179=(
REPRESENTATION_RELATIONSHIP($,$,#11746,#11722)
REPRESENTATION_RELATIONSHIP_WITH_TRANSFORMATION(#94)
SHAPE_REPRESENTATION_RELATIONSHIP()
);
#180=(
REPRESENTATION_RELATIONSHIP($,$,#11745,#11722)
REPRESENTATION_RELATIONSHIP_WITH_TRANSFORMATION(#95)
SHAPE_REPRESENTATION_RELATIONSHIP()
);
#181=(
REPRESENTATION_RELATIONSHIP($,$,#11746,#11722)
REPRESENTATION_RELATIONSHIP_WITH_TRANSFORMATION(#96)
SHAPE_REPRESENTATION_RELATIONSHIP()
);
#182=(
REPRESENTATION_RELATIONSHIP($,$,#11747,#11722)
REPRESENTATION_RELATIONSHIP_WITH_TRANSFORMATION(#97)
SHAPE_REPRESENTATION_RELATIONSHIP()
);
#183=(
REPRESENTATION_RELATIONSHIP($,$,#11749,#11748)
REPRESENTATION_RELATIONSHIP_WITH_TRANSFORMATION(#98)
SHAPE_REPRESENTATION_RELATIONSHIP()
);
#184=(
REPRESENTATION_RELATIONSHIP($,$,#11750,#11748)
REPRESENTATION_RELATIONSHIP_WITH_TRANSFORMATION(#99)
SHAPE_REPRESENTATION_RELATIONSHIP()
);
#185=(
REPRESENTATION_RELATIONSHIP($,$,#11751,#11748)
REPRESENTATION_RELATIONSHIP_WITH_TRANSFORMATION(#100)
SHAPE_REPRESENTATION_RELATIONSHIP()
);
#186=(
REPRESENTATION_RELATIONSHIP($,$,#11752,#11748)
REPRESENTATION_RELATIONSHIP_WITH_TRANSFORMATION(#101)
SHAPE_REPRESENTATION_RELATIONSHIP()
);
#187=(
REPRESENTATION_RELATIONSHIP($,$,#11753,#11748)
REPRESENTATION_RELATIONSHIP_WITH_TRANSFORMATION(#102)
SHAPE_REPRESENTATION_RELATIONSHIP()
);
#188=(
REPRESENTATION_RELATIONSHIP($,$,#11754,#11748)
REPRESENTATION_RELATIONSHIP_WITH_TRANSFORMATION(#103)
SHAPE_REPRESENTATION_RELATIONSHIP()
);
#189=(
REPRESENTATION_RELATIONSHIP($,$,#11755,#11748)
REPRESENTATION_RELATIONSHIP_WITH_TRANSFORMATION(#104)
SHAPE_REPRESENTATION_RELATIONSHIP()
);
#190=(
REPRESENTATION_RELATIONSHIP($,$,#11756,#11748)
REPRESENTATION_RELATIONSHIP_WITH_TRANSFORMATION(#105)
SHAPE_REPRESENTATION_RELATIONSHIP()
);
#191=(
REPRESENTATION_RELATIONSHIP($,$,#11722,#11721)
REPRESENTATION_RELATIONSHIP_WITH_TRANSFORMATION(#106)
SHAPE_REPRESENTATION_RELATIONSHIP()
);
#192=(
REPRESENTATION_RELATIONSHIP($,$,#11748,#11721)
REPRESENTATION_RELATIONSHIP_WITH_TRANSFORMATION(#107)
SHAPE_REPRESENTATION_RELATIONSHIP()
);
#193=CONTEXT_DEPENDENT_SHAPE_REPRESENTATION(#108,#11624);
#194=CONTEXT_DEPENDENT_SHAPE_REPRESENTATION(#109,#11625);
#195=CONTEXT_DEPENDENT_SHAPE_REPRESENTATION(#110,#11629);
#196=CONTEXT_DEPENDENT_SHAPE_REPRESENTATION(#111,#11630);
#197=CONTEXT_DEPENDENT_SHAPE_REPRESENTATION(#112,#11631);
#198=CONTEXT_DEPENDENT_SHAPE_REPRESENTATION(#113,#11632);
#199=CONTEXT_DEPENDENT_SHAPE_REPRESENTATION(#114,#11633);
#200=CONTEXT_DEPENDENT_SHAPE_REPRESENTATION(#115,#11634);
#201=CONTEXT_DEPENDENT_SHAPE_REPRESENTATION(#116,#11635);
#202=CONTEXT_DEPENDENT_SHAPE_REPRESENTATION(#117,#11636);
#203=CONTEXT_DEPENDENT_SHAPE_REPRESENTATION(#118,#11637);
#204=CONTEXT_DEPENDENT_SHAPE_REPRESENTATION(#119,#11638);
#205=CONTEXT_DEPENDENT_SHAPE_REPRESENTATION(#120,#11639);
#206=CONTEXT_DEPENDENT_SHAPE_REPRESENTATION(#121,#11640);
#207=CONTEXT_DEPENDENT_SHAPE_REPRESENTATION(#122,#11641);
#208=CONTEXT_DEPENDENT_SHAPE_REPRESENTATION(#123,#11642);
#209=CONTEXT_DEPENDENT_SHAPE_REPRESENTATION(#124,#11643);
#210=CONTEXT_DEPENDENT_SHAPE_REPRESENTATION(#125,#11644);
#211=CONTEXT_DEPENDENT_SHAPE_REPRESENTATION(#126,#11645);
#212=CONTEXT_DEPENDENT_SHAPE_REPRESENTATION(#127,#11646);
#213=CONTEXT_DEPENDENT_SHAPE_REPRESENTATION(#128,#11647);
#214=CONTEXT_DEPENDENT_SHAPE_REPRESENTATION(#129,#11648);
#215=CONTEXT_DEPENDENT_SHAPE_REPRESENTATION(#130,#11649);
#216=CONTEXT_DEPENDENT_SHAPE_REPRESENTATION(#131,#11650);
#217=CONTEXT_DEPENDENT_SHAPE_REPRESENTATION(#132,#11651);
#218=CONTEXT_DEPENDENT_SHAPE_REPRESENTATION(#133,#11652);
#219=CONTEXT_DEPENDENT_SHAPE_REPRESENTATION(#134,#11653);
#220=CONTEXT_DEPENDENT_SHAPE_REPRESENTATION(#135,#11654);
#221=CONTEXT_DEPENDENT_SHAPE_REPRESENTATION(#136,#11655);
#222=CONTEXT_DEPENDENT_SHAPE_REPRESENTATION(#137,#11656);
#223=CONTEXT_DEPENDENT_SHAPE_REPRESENTATION(#138,#11657);
#224=CONTEXT_DEPENDENT_SHAPE_REPRESENTATION(#139,#11658);
#225=CONTEXT_DEPENDENT_SHAPE_REPRESENTATION(#140,#11659);
#226=CONTEXT_DEPENDENT_SHAPE_REPRESENTATION(#141,#11660);
#227=CONTEXT_DEPENDENT_SHAPE_REPRESENTATION(#142,#11661);
#228=CONTEXT_DEPENDENT_SHAPE_REPRESENTATION(#143,#11662);
#229=CONTEXT_DEPENDENT_SHAPE_REPRESENTATION(#144,#11663);
#230=CONTEXT_DEPENDENT_SHAPE_REPRESENTATION(#145,#11664);
#231=CONTEXT_DEPENDENT_SHAPE_REPRESENTATION(#146,#11665);
#232=CONTEXT_DEPENDENT_SHAPE_REPRESENTATION(#147,#11666);
#233=CONTEXT_DEPENDENT_SHAPE_REPRESENTATION(#148,#11667);
#234=CONTEXT_DEPENDENT_SHAPE_REPRESENTATION(#149,#11668);
#235=CONTEXT_DEPENDENT_SHAPE_REPRESENTATION(#150,#11669);
#236=CONTEXT_DEPENDENT_SHAPE_REPRESENTATION(#151,#11670);
#237=CONTEXT_DEPENDENT_SHAPE_REPRESENTATION(#152,#11671);
#238=CONTEXT_DEPENDENT_SHAPE_REPRESENTATION(#153,#11672);
#239=CONTEXT_DEPENDENT_SHAPE_REPRESENTATION(#154,#11673);
#240=CONTEXT_DEPENDENT_SHAPE_REPRESENTATION(#155,#11674);
#241=CONTEXT_DEPENDENT_SHAPE_REPRESENTATION(#156,#11675);
#242=CONTEXT_DEPENDENT_SHAPE_REPRESENTATION(#157,#11676);
#243=CONTEXT_DEPENDENT_SHAPE_REPRESENTATION(#158,#11677);
#244=CONTEXT_DEPENDENT_SHAPE_REPRESENTATION(#159,#11678);
#245=CONTEXT_DEPENDENT_SHAPE_REPRESENTATION(#160,#11679);
#246=CONTEXT_DEPENDENT_SHAPE_REPRESENTATION(#161,#11680);
#247=CONTEXT_DEPENDENT_SHAPE_REPRESENTATION(#162,#11681);
#248=CONTEXT_DEPENDENT_SHAPE_REPRESENTATION(#163,#11682);
#249=CONTEXT_DEPENDENT_SHAPE_REPRESENTATION(#164,#11683);
#250=CONTEXT_DEPENDENT_SHAPE_REPRESENTATION(#165,#11684);
#251=CONTEXT_DEPENDENT_SHAPE_REPRESENTATION(#166,#11685);
#252=CONTEXT_DEPENDENT_SHAPE_REPRESENTATION(#167,#11686);
#253=CONTEXT_DEPENDENT_SHAPE_REPRESENTATION(#168,#11687);
#254=CONTEXT_DEPENDENT_SHAPE_REPRESENTATION(#169,#11688);
#255=CONTEXT_DEPENDENT_SHAPE_REPRESENTATION(#170,#11689);
#256=CONTEXT_DEPENDENT_SHAPE_REPRESENTATION(#171,#11690);
#257=CONTEXT_DEPENDENT_SHAPE_REPRESENTATION(#172,#11691);
#258=CONTEXT_DEPENDENT_SHAPE_REPRESENTATION(#173,#11692);
#259=CONTEXT_DEPENDENT_SHAPE_REPRESENTATION(#174,#11693);
#260=CONTEXT_DEPENDENT_SHAPE_REPRESENTATION(#175,#11694);
#261=CONTEXT_DEPENDENT_SHAPE_REPRESENTATION(#176,#11695);
#262=CONTEXT_DEPENDENT_SHAPE_REPRESENTATION(#177,#11696);
#263=CONTEXT_DEPENDENT_SHAPE_REPRESENTATION(#178,#11697);
#264=CONTEXT_DEPENDENT_SHAPE_REPRESENTATION(#179,#11698);
#265=CONTEXT_DEPENDENT_SHAPE_REPRESENTATION(#180,#11699);
#266=CONTEXT_DEPENDENT_SHAPE_REPRESENTATION(#181,#11700);
#267=CONTEXT_DEPENDENT_SHAPE_REPRESENTATION(#182,#11701);
#268=CONTEXT_DEPENDENT_SHAPE_REPRESENTATION(#183,#11711);
#269=CONTEXT_DEPENDENT_SHAPE_REPRESENTATION(#184,#11712);
#270=CONTEXT_DEPENDENT_SHAPE_REPRESENTATION(#185,#11713);
#271=CONTEXT_DEPENDENT_SHAPE_REPRESENTATION(#186,#11714);
#272=CONTEXT_DEPENDENT_SHAPE_REPRESENTATION(#187,#11715);
#273=CONTEXT_DEPENDENT_SHAPE_REPRESENTATION(#188,#11716);
#274=CONTEXT_DEPENDENT_SHAPE_REPRESENTATION(#189,#11717);
#275=CONTEXT_DEPENDENT_SHAPE_REPRESENTATION(#190,#11718);
#276=CONTEXT_DEPENDENT_SHAPE_REPRESENTATION(#191,#11719);
#277=CONTEXT_DEPENDENT_SHAPE_REPRESENTATION(#192,#11720);
#278=NEXT_ASSEMBLY_USAGE_OCCURRENCE('Housing:1','Housing:1','Housing:1',
#11779,#11780,'Housing:1');
#279=NEXT_ASSEMBLY_USAGE_OCCURRENCE('Insert bearing:1',
'Insert bearing:1','Insert bearing:1',#11779,#11781,'Insert bearing:1');
#280=NEXT_ASSEMBLY_USAGE_OCCURRENCE('Base plate:1','Base plate:1',
'Base plate:1',#11759,#11760,'Base plate:1');
#281=NEXT_ASSEMBLY_USAGE_OCCURRENCE('Bonded foot pad:1',
'Bonded foot pad:1','Bonded foot pad:1',#11759,#11761,
'Bonded foot pad:1');
#282=NEXT_ASSEMBLY_USAGE_OCCURRENCE('Bonded foot pad (1):1',
'Bonded foot pad (1):1','Bonded foot pad (1):1',#11759,#11762,
'Bonded foot pad (1):1');
#283=NEXT_ASSEMBLY_USAGE_OCCURRENCE('Bonded foot pad (2):1',
'Bonded foot pad (2):1','Bonded foot pad (2):1',#11759,#11763,
'Bonded foot pad (2):1');
#284=NEXT_ASSEMBLY_USAGE_OCCURRENCE('Bonded foot pad (3):1',
'Bonded foot pad (3):1','Bonded foot pad (3):1',#11759,#11764,
'Bonded foot pad (3):1');
#285=NEXT_ASSEMBLY_USAGE_OCCURRENCE('Flange adapter:1',
'Flange adapter:1','Flange adapter:1',#11759,#11765,'Flange adapter:1');
#286=NEXT_ASSEMBLY_USAGE_OCCURRENCE('Flange hole reducer:1',
'Flange hole reducer:1','Flange hole reducer:1',#11759,#11766,
'Flange hole reducer:1');
#287=NEXT_ASSEMBLY_USAGE_OCCURRENCE('Flange hole reducer (1):1',
'Flange hole reducer (1):1','Flange hole reducer (1):1',#11759,#11767,
'Flange hole reducer (1):1');
#288=NEXT_ASSEMBLY_USAGE_OCCURRENCE('Flange hole reducer (2):1',
'Flange hole reducer (2):1','Flange hole reducer (2):1',#11759,#11768,
'Flange hole reducer (2):1');
#289=NEXT_ASSEMBLY_USAGE_OCCURRENCE('Flange hole reducer (3):1',
'Flange hole reducer (3):1','Flange hole reducer (3):1',#11759,#11769,
'Flange hole reducer (3):1');
#290=NEXT_ASSEMBLY_USAGE_OCCURRENCE('Flange adapter (1):1',
'Flange adapter (1):1','Flange adapter (1):1',#11759,#11770,
'Flange adapter (1):1');
#291=NEXT_ASSEMBLY_USAGE_OCCURRENCE('Flange hole reducer (4):1',
'Flange hole reducer (4):1','Flange hole reducer (4):1',#11759,#11771,
'Flange hole reducer (4):1');
#292=NEXT_ASSEMBLY_USAGE_OCCURRENCE('Flange hole reducer (5):1',
'Flange hole reducer (5):1','Flange hole reducer (5):1',#11759,#11772,
'Flange hole reducer (5):1');
#293=NEXT_ASSEMBLY_USAGE_OCCURRENCE('Flange hole reducer (6):1',
'Flange hole reducer (6):1','Flange hole reducer (6):1',#11759,#11773,
'Flange hole reducer (6):1');
#294=NEXT_ASSEMBLY_USAGE_OCCURRENCE('Flange hole reducer (7):1',
'Flange hole reducer (7):1','Flange hole reducer (7):1',#11759,#11774,
'Flange hole reducer (7):1');
#295=NEXT_ASSEMBLY_USAGE_OCCURRENCE(
'Slotted Extrusion - 20 x 20 x 200 mm:2',
'Slotted Extrusion - 20 x 20 x 200 mm:2',
'Slotted Extrusion - 20 x 20 x 200 mm:2',#11759,#11775,
'Slotted Extrusion - 20 x 20 x 200 mm:2');
#296=NEXT_ASSEMBLY_USAGE_OCCURRENCE('Captive slot nut:2',
'Captive slot nut:2','Captive slot nut:2',#11759,#11776,
'Captive slot nut:2');
#297=NEXT_ASSEMBLY_USAGE_OCCURRENCE('M5x17 screw:2','M5x17 screw:2',
'M5x17 screw:2',#11759,#11777,'M5x17 screw:2');
#298=NEXT_ASSEMBLY_USAGE_OCCURRENCE('Captive slot nut:3',
'Captive slot nut:3','Captive slot nut:3',#11759,#11776,
'Captive slot nut:3');
#299=NEXT_ASSEMBLY_USAGE_OCCURRENCE('M5x17 screw:3','M5x17 screw:3',
'M5x17 screw:3',#11759,#11777,'M5x17 screw:3');
#300=NEXT_ASSEMBLY_USAGE_OCCURRENCE(
'Slotted Extrusion - 20 x 20 x 200 mm:3',
'Slotted Extrusion - 20 x 20 x 200 mm:3',
'Slotted Extrusion - 20 x 20 x 200 mm:3',#11759,#11775,
'Slotted Extrusion - 20 x 20 x 200 mm:3');
#301=NEXT_ASSEMBLY_USAGE_OCCURRENCE('Captive slot nut:4',
'Captive slot nut:4','Captive slot nut:4',#11759,#11776,
'Captive slot nut:4');
#302=NEXT_ASSEMBLY_USAGE_OCCURRENCE('M5x17 screw:4','M5x17 screw:4',
'M5x17 screw:4',#11759,#11777,'M5x17 screw:4');
#303=NEXT_ASSEMBLY_USAGE_OCCURRENCE('Captive slot nut:5',
'Captive slot nut:5','Captive slot nut:5',#11759,#11776,
'Captive slot nut:5');
#304=NEXT_ASSEMBLY_USAGE_OCCURRENCE('M5x17 screw:5','M5x17 screw:5',
'M5x17 screw:5',#11759,#11777,'M5x17 screw:5');
#305=NEXT_ASSEMBLY_USAGE_OCCURRENCE(
'Slotted Extrusion - 20 x 20 x 200 mm:4',
'Slotted Extrusion - 20 x 20 x 200 mm:4',
'Slotted Extrusion - 20 x 20 x 200 mm:4',#11759,#11775,
'Slotted Extrusion - 20 x 20 x 200 mm:4');
#306=NEXT_ASSEMBLY_USAGE_OCCURRENCE('Captive slot nut:6',
'Captive slot nut:6','Captive slot nut:6',#11759,#11776,
'Captive slot nut:6');
#307=NEXT_ASSEMBLY_USAGE_OCCURRENCE('M5x17 screw:6','M5x17 screw:6',
'M5x17 screw:6',#11759,#11777,'M5x17 screw:6');
#308=NEXT_ASSEMBLY_USAGE_OCCURRENCE('Captive slot nut:7',
'Captive slot nut:7','Captive slot nut:7',#11759,#11776,
'Captive slot nut:7');
#309=NEXT_ASSEMBLY_USAGE_OCCURRENCE('M5x17 screw:7','M5x17 screw:7',
'M5x17 screw:7',#11759,#11777,'M5x17 screw:7');
#310=NEXT_ASSEMBLY_USAGE_OCCURRENCE(
'Slotted Extrusion - 20 x 20 x 200 mm:5',
'Slotted Extrusion - 20 x 20 x 200 mm:5',
'Slotted Extrusion - 20 x 20 x 200 mm:5',#11759,#11775,
'Slotted Extrusion - 20 x 20 x 200 mm:5');
#311=NEXT_ASSEMBLY_USAGE_OCCURRENCE('Captive slot nut:8',
'Captive slot nut:8','Captive slot nut:8',#11759,#11776,
'Captive slot nut:8');
#312=NEXT_ASSEMBLY_USAGE_OCCURRENCE('M5x17 screw:8','M5x17 screw:8',
'M5x17 screw:8',#11759,#11777,'M5x17 screw:8');
#313=NEXT_ASSEMBLY_USAGE_OCCURRENCE('Captive slot nut:9',
'Captive slot nut:9','Captive slot nut:9',#11759,#11776,
'Captive slot nut:9');
#314=NEXT_ASSEMBLY_USAGE_OCCURRENCE('M5x17 screw:9','M5x17 screw:9',
'M5x17 screw:9',#11759,#11777,'M5x17 screw:9');
#315=NEXT_ASSEMBLY_USAGE_OCCURRENCE('M6x18 mounting screw:2',
'M6x18 mounting screw:2','M6x18 mounting screw:2',#11759,#11778,
'M6x18 mounting screw:2');
#316=NEXT_ASSEMBLY_USAGE_OCCURRENCE('M6x18 mounting screw:3',
'M6x18 mounting screw:3','M6x18 mounting screw:3',#11759,#11778,
'M6x18 mounting screw:3');
#317=NEXT_ASSEMBLY_USAGE_OCCURRENCE(
'Square Flange Bearing - 12 mm Bore:2',
'Square Flange Bearing - 12 mm Bore:2',
'Square Flange Bearing - 12 mm Bore:2',#11759,#11779,
'Square Flange Bearing - 12 mm Bore:2');
#318=NEXT_ASSEMBLY_USAGE_OCCURRENCE('Flat Washer - M8:2',
'Flat Washer - M8:2','Flat Washer - M8:2',#11759,#11783,
'Flat Washer - M8:2');
#319=NEXT_ASSEMBLY_USAGE_OCCURRENCE('Cap Screw - M8x30:2',
'Cap Screw - M8x30:2','Cap Screw - M8x30:2',#11759,#11782,
'Cap Screw - M8x30:2');
#320=NEXT_ASSEMBLY_USAGE_OCCURRENCE('Flat Washer - M8:3',
'Flat Washer - M8:3','Flat Washer - M8:3',#11759,#11783,
'Flat Washer - M8:3');
#321=NEXT_ASSEMBLY_USAGE_OCCURRENCE('Hex Nut - M8:2','Hex Nut - M8:2',
'Hex Nut - M8:2',#11759,#11784,'Hex Nut - M8:2');
#322=NEXT_ASSEMBLY_USAGE_OCCURRENCE('Flat Washer - M8:4',
'Flat Washer - M8:4','Flat Washer - M8:4',#11759,#11783,
'Flat Washer - M8:4');
#323=NEXT_ASSEMBLY_USAGE_OCCURRENCE('Cap Screw - M8x30:3',
'Cap Screw - M8x30:3','Cap Screw - M8x30:3',#11759,#11782,
'Cap Screw - M8x30:3');
#324=NEXT_ASSEMBLY_USAGE_OCCURRENCE('Flat Washer - M8:5',
'Flat Washer - M8:5','Flat Washer - M8:5',#11759,#11783,
'Flat Washer - M8:5');
#325=NEXT_ASSEMBLY_USAGE_OCCURRENCE('Hex Nut - M8:3','Hex Nut - M8:3',
'Hex Nut - M8:3',#11759,#11784,'Hex Nut - M8:3');
#326=NEXT_ASSEMBLY_USAGE_OCCURRENCE('Flat Washer - M8:6',
'Flat Washer - M8:6','Flat Washer - M8:6',#11759,#11783,
'Flat Washer - M8:6');
#327=NEXT_ASSEMBLY_USAGE_OCCURRENCE('Cap Screw - M8x30:4',
'Cap Screw - M8x30:4','Cap Screw - M8x30:4',#11759,#11782,
'Cap Screw - M8x30:4');
#328=NEXT_ASSEMBLY_USAGE_OCCURRENCE('Flat Washer - M8:7',
'Flat Washer - M8:7','Flat Washer - M8:7',#11759,#11783,
'Flat Washer - M8:7');
#329=NEXT_ASSEMBLY_USAGE_OCCURRENCE('Hex Nut - M8:4','Hex Nut - M8:4',
'Hex Nut - M8:4',#11759,#11784,'Hex Nut - M8:4');
#330=NEXT_ASSEMBLY_USAGE_OCCURRENCE('Flat Washer - M8:8',
'Flat Washer - M8:8','Flat Washer - M8:8',#11759,#11783,
'Flat Washer - M8:8');
#331=NEXT_ASSEMBLY_USAGE_OCCURRENCE('Cap Screw - M8x30:5',
'Cap Screw - M8x30:5','Cap Screw - M8x30:5',#11759,#11782,
'Cap Screw - M8x30:5');
#332=NEXT_ASSEMBLY_USAGE_OCCURRENCE('Flat Washer - M8:9',
'Flat Washer - M8:9','Flat Washer - M8:9',#11759,#11783,
'Flat Washer - M8:9');
#333=NEXT_ASSEMBLY_USAGE_OCCURRENCE('Hex Nut - M8:5','Hex Nut - M8:5',
'Hex Nut - M8:5',#11759,#11784,'Hex Nut - M8:5');
#334=NEXT_ASSEMBLY_USAGE_OCCURRENCE('M6x18 mounting screw:4',
'M6x18 mounting screw:4','M6x18 mounting screw:4',#11759,#11778,
'M6x18 mounting screw:4');
#335=NEXT_ASSEMBLY_USAGE_OCCURRENCE('M6x18 mounting screw:5',
'M6x18 mounting screw:5','M6x18 mounting screw:5',#11759,#11778,
'M6x18 mounting screw:5');
#336=NEXT_ASSEMBLY_USAGE_OCCURRENCE(
'Square Flange Bearing - 12 mm Bore:3',
'Square Flange Bearing - 12 mm Bore:3',
'Square Flange Bearing - 12 mm Bore:3',#11759,#11779,
'Square Flange Bearing - 12 mm Bore:3');
#337=NEXT_ASSEMBLY_USAGE_OCCURRENCE('Flat Washer - M8:10',
'Flat Washer - M8:10','Flat Washer - M8:10',#11759,#11783,
'Flat Washer - M8:10');
#338=NEXT_ASSEMBLY_USAGE_OCCURRENCE('Cap Screw - M8x30:6',
'Cap Screw - M8x30:6','Cap Screw - M8x30:6',#11759,#11782,
'Cap Screw - M8x30:6');
#339=NEXT_ASSEMBLY_USAGE_OCCURRENCE('Flat Washer - M8:11',
'Flat Washer - M8:11','Flat Washer - M8:11',#11759,#11783,
'Flat Washer - M8:11');
#340=NEXT_ASSEMBLY_USAGE_OCCURRENCE('Hex Nut - M8:6','Hex Nut - M8:6',
'Hex Nut - M8:6',#11759,#11784,'Hex Nut - M8:6');
#341=NEXT_ASSEMBLY_USAGE_OCCURRENCE('Flat Washer - M8:12',
'Flat Washer - M8:12','Flat Washer - M8:12',#11759,#11783,
'Flat Washer - M8:12');
#342=NEXT_ASSEMBLY_USAGE_OCCURRENCE('Cap Screw - M8x30:7',
'Cap Screw - M8x30:7','Cap Screw - M8x30:7',#11759,#11782,
'Cap Screw - M8x30:7');
#343=NEXT_ASSEMBLY_USAGE_OCCURRENCE('Flat Washer - M8:13',
'Flat Washer - M8:13','Flat Washer - M8:13',#11759,#11783,
'Flat Washer - M8:13');
#344=NEXT_ASSEMBLY_USAGE_OCCURRENCE('Hex Nut - M8:7','Hex Nut - M8:7',
'Hex Nut - M8:7',#11759,#11784,'Hex Nut - M8:7');
#345=NEXT_ASSEMBLY_USAGE_OCCURRENCE('Flat Washer - M8:14',
'Flat Washer - M8:14','Flat Washer - M8:14',#11759,#11783,
'Flat Washer - M8:14');
#346=NEXT_ASSEMBLY_USAGE_OCCURRENCE('Cap Screw - M8x30:8',
'Cap Screw - M8x30:8','Cap Screw - M8x30:8',#11759,#11782,
'Cap Screw - M8x30:8');
#347=NEXT_ASSEMBLY_USAGE_OCCURRENCE('Flat Washer - M8:15',
'Flat Washer - M8:15','Flat Washer - M8:15',#11759,#11783,
'Flat Washer - M8:15');
#348=NEXT_ASSEMBLY_USAGE_OCCURRENCE('Hex Nut - M8:8','Hex Nut - M8:8',
'Hex Nut - M8:8',#11759,#11784,'Hex Nut - M8:8');
#349=NEXT_ASSEMBLY_USAGE_OCCURRENCE('Flat Washer - M8:16',
'Flat Washer - M8:16','Flat Washer - M8:16',#11759,#11783,
'Flat Washer - M8:16');
#350=NEXT_ASSEMBLY_USAGE_OCCURRENCE('Cap Screw - M8x30:9',
'Cap Screw - M8x30:9','Cap Screw - M8x30:9',#11759,#11782,
'Cap Screw - M8x30:9');
#351=NEXT_ASSEMBLY_USAGE_OCCURRENCE('Flat Washer - M8:17',
'Flat Washer - M8:17','Flat Washer - M8:17',#11759,#11783,
'Flat Washer - M8:17');
#352=NEXT_ASSEMBLY_USAGE_OCCURRENCE('Hex Nut - M8:9','Hex Nut - M8:9',
'Hex Nut - M8:9',#11759,#11784,'Hex Nut - M8:9');
#353=NEXT_ASSEMBLY_USAGE_OCCURRENCE('Shaft:1','Shaft:1','Shaft:1',#11785,
#11786,'Shaft:1');
#354=NEXT_ASSEMBLY_USAGE_OCCURRENCE('Rear thrust spacer:1',
'Rear thrust spacer:1','Rear thrust spacer:1',#11785,#11787,
'Rear thrust spacer:1');
#355=NEXT_ASSEMBLY_USAGE_OCCURRENCE('Front thrust spacer:1',
'Front thrust spacer:1','Front thrust spacer:1',#11785,#11788,
'Front thrust spacer:1');
#356=NEXT_ASSEMBLY_USAGE_OCCURRENCE('Adjustment nut:1',
'Adjustment nut:1','Adjustment nut:1',#11785,#11789,'Adjustment nut:1');
#357=NEXT_ASSEMBLY_USAGE_OCCURRENCE('Jam nut:1','Jam nut:1','Jam nut:1',
#11785,#11790,'Jam nut:1');
#358=NEXT_ASSEMBLY_USAGE_OCCURRENCE('Drive hub:1','Drive hub:1',
'Drive hub:1',#11785,#11791,'Drive hub:1');
#359=NEXT_ASSEMBLY_USAGE_OCCURRENCE('Key 4x4x14:2','Key 4x4x14:2',
'Key 4x4x14:2',#11785,#11792,'Key 4x4x14:2');
#360=NEXT_ASSEMBLY_USAGE_OCCURRENCE('Socket Set Screw - M5x8:2',
'Socket Set Screw - M5x8:2','Socket Set Screw - M5x8:2',#11785,#11793,
'Socket Set Screw - M5x8:2');
#361=NEXT_ASSEMBLY_USAGE_OCCURRENCE('Extrusion support frame:1',
'Extrusion support frame:1','Extrusion support frame:1',#11758,#11759,
'Extrusion support frame:1');
#362=NEXT_ASSEMBLY_USAGE_OCCURRENCE('Shaft and axial retention:1',
'Shaft and axial retention:1','Shaft and axial retention:1',#11758,#11785,
'Shaft and axial retention:1');
#363=B_SPLINE_CURVE_WITH_KNOTS('',3,(#10336,#10337,#10338,#10339,#10340,
#10341,#10342,#10343,#10344,#10345),.UNSPECIFIED.,.F.,.F.,(4,2,2,2,4),(1.13193471301885,
1.22626174930539,1.32058878559194,1.41491753480854,1.50924628402513),
 .UNSPECIFIED.);
#364=B_SPLINE_CURVE_WITH_KNOTS('',3,(#10347,#10348,#10349,#10350,#10351,
#10352,#10353,#10354,#10355,#10356,#10357,#10358,#10359,#10360,#10361,#10362,
#10363,#10364),.UNSPECIFIED.,.F.,.F.,(4,2,2,2,2,2,2,2,4),(0.377311571006283,
0.471638607292829,0.565965643579376,0.66029439279597,0.754623142012565,
0.84895189122916,0.943280640445754,1.0376076767323,1.13193471301885),
 .UNSPECIFIED.);
#365=B_SPLINE_CURVE_WITH_KNOTS('',3,(#10365,#10366,#10367,#10368,#10369,
#10370,#10371,#10372,#10373,#10374),.UNSPECIFIED.,.F.,.F.,(4,2,2,2,4),(1.50924628402513,
1.60357503324173,1.69790378245832,1.79223081874487,1.88655785503141),
 .UNSPECIFIED.);
#366=B_SPLINE_CURVE_WITH_KNOTS('',3,(#10377,#10378,#10379,#10380,#10381,
#10382,#10383,#10384,#10385,#10386,#10387,#10388,#10389,#10390,#10391,#10392,
#10393,#10394,#10395,#10396,#10397,#10398,#10399,#10400,#10401,#10402,#10403,
#10404,#10405,#10406,#10407,#10408,#10409,#10410),.UNSPECIFIED.,.T.,.F.,
(4,2,2,2,2,2,2,2,2,2,2,2,2,2,2,2,4),(0.,0.0955080856649705,0.191016171329941,
0.286408845249646,0.38180151916935,0.477194193089055,0.572586867008759,
0.66809495267373,0.763603038338701,0.859111124003671,0.954619209668642,
1.05001188358835,1.14540455750805,1.24079723142776,1.33618990534746,1.43169799101243,
1.5272060766774),.UNSPECIFIED.);
#367=B_SPLINE_CURVE_WITH_KNOTS('',3,(#10413,#10414,#10415,#10416,#10417,
#10418,#10419,#10420,#10421,#10422,#10423,#10424,#10425,#10426,#10427,#10428,
#10429,#10430,#10431,#10432,#10433,#10434,#10435,#10436,#10437,#10438,#10439,
#10440,#10441,#10442,#10443,#10444,#10445,#10446),.UNSPECIFIED.,.T.,.F.,
(4,2,2,2,2,2,2,2,2,2,2,2,2,2,2,2,4),(0.,0.0955080856649706,0.191016171329941,
0.286408845249646,0.381801519169351,0.477194193089055,0.57258686700876,
0.668094952673731,0.763603038338701,0.859111124003672,0.954619209668642,
1.05001188358835,1.14540455750805,1.24079723142776,1.33618990534746,1.43169799101243,
1.5272060766774),.UNSPECIFIED.);
#368=B_SPLINE_CURVE_WITH_KNOTS('',3,(#10450,#10451,#10452,#10453,#10454,
#10455,#10456,#10457,#10458,#10459),.UNSPECIFIED.,.F.,.F.,(4,2,2,2,4),(1.13193471301885,
1.22626174930539,1.32058878559194,1.41491753480854,1.50924628402513),
 .UNSPECIFIED.);
#369=B_SPLINE_CURVE_WITH_KNOTS('',3,(#10461,#10462,#10463,#10464,#10465,
#10466,#10467,#10468,#10469,#10470,#10471,#10472,#10473,#10474,#10475,#10476,
#10477,#10478),.UNSPECIFIED.,.F.,.F.,(4,2,2,2,2,2,2,2,4),(0.377311571006283,
0.47163860729283,0.565965643579376,0.660294392795971,0.754623142012565,
0.84895189122916,0.943280640445755,1.0376076767323,1.13193471301885),
 .UNSPECIFIED.);
#370=B_SPLINE_CURVE_WITH_KNOTS('',3,(#10479,#10480,#10481,#10482,#10483,
#10484,#10485,#10486,#10487,#10488),.UNSPECIFIED.,.F.,.F.,(4,2,2,2,4),(1.50924628402513,
1.60357503324173,1.69790378245832,1.79223081874487,1.88655785503141),
 .UNSPECIFIED.);
#371=B_SPLINE_CURVE_WITH_KNOTS('',3,(#10497,#10498,#10499,#10500,#10501,
#10502,#10503,#10504,#10505,#10506,#10507,#10508,#10509,#10510,#10511,#10512,
#10513,#10514),.UNSPECIFIED.,.F.,.F.,(4,2,2,2,2,2,2,2,4),(0.377311571006282,
0.471638607292829,0.565965643579376,0.660294392795971,0.754623142012565,
0.84895189122916,0.943280640445754,1.0376076767323,1.13193471301885),
 .UNSPECIFIED.);
#372=B_SPLINE_CURVE_WITH_KNOTS('',3,(#10516,#10517,#10518,#10519,#10520,
#10521,#10522,#10523,#10524,#10525),.UNSPECIFIED.,.F.,.F.,(4,2,2,2,4),(1.13193471301885,
1.22626174930539,1.32058878559194,1.41491753480854,1.50924628402513),
 .UNSPECIFIED.);
#373=B_SPLINE_CURVE_WITH_KNOTS('',3,(#10526,#10527,#10528,#10529,#10530,
#10531,#10532,#10533,#10534,#10535),.UNSPECIFIED.,.F.,.F.,(4,2,2,2,4),(1.50924628402513,
1.60357503324172,1.69790378245832,1.79223081874487,1.88655785503141),
 .UNSPECIFIED.);
#374=B_SPLINE_CURVE_WITH_KNOTS('',3,(#10538,#10539,#10540,#10541,#10542,
#10543,#10544,#10545,#10546,#10547,#10548,#10549,#10550,#10551,#10552,#10553,
#10554,#10555),.UNSPECIFIED.,.F.,.F.,(4,2,2,2,2,2,2,2,4),(0.377311571006283,
0.47163860729283,0.565965643579376,0.660294392795971,0.754623142012565,
0.84895189122916,0.943280640445754,1.0376076767323,1.13193471301885),
 .UNSPECIFIED.);
#375=B_SPLINE_CURVE_WITH_KNOTS('',3,(#10557,#10558,#10559,#10560,#10561,
#10562,#10563,#10564,#10565,#10566),.UNSPECIFIED.,.F.,.F.,(4,2,2,2,4),(1.13193471301885,
1.22626174930539,1.32058878559194,1.41491753480854,1.50924628402513),
 .UNSPECIFIED.);
#376=B_SPLINE_CURVE_WITH_KNOTS('',3,(#10567,#10568,#10569,#10570,#10571,
#10572,#10573,#10574,#10575,#10576),.UNSPECIFIED.,.F.,.F.,(4,2,2,2,4),(1.50924628402513,
1.60357503324173,1.69790378245832,1.79223081874487,1.88655785503141),
 .UNSPECIFIED.);
#377=B_SPLINE_CURVE_WITH_KNOTS('',3,(#10579,#10580,#10581,#10582,#10583,
#10584,#10585,#10586,#10587,#10588,#10589,#10590,#10591,#10592,#10593,#10594,
#10595,#10596),.UNSPECIFIED.,.F.,.F.,(4,2,2,2,2,2,2,2,4),(0.377311571006282,
0.471638607292829,0.565965643579376,0.66029439279597,0.754623142012565,
0.84895189122916,0.943280640445754,1.0376076767323,1.13193471301885),
 .UNSPECIFIED.);
#378=B_SPLINE_CURVE_WITH_KNOTS('',3,(#10598,#10599,#10600,#10601,#10602,
#10603,#10604,#10605,#10606,#10607),.UNSPECIFIED.,.F.,.F.,(4,2,2,2,4),(1.13193471301885,
1.22626174930539,1.32058878559194,1.41491753480854,1.50924628402513),
 .UNSPECIFIED.);
#379=B_SPLINE_CURVE_WITH_KNOTS('',3,(#10608,#10609,#10610,#10611,#10612,
#10613,#10614,#10615,#10616,#10617),.UNSPECIFIED.,.F.,.F.,(4,2,2,2,4),(1.50924628402513,
1.60357503324172,1.69790378245832,1.79223081874487,1.88655785503141),
 .UNSPECIFIED.);
#380=B_SPLINE_CURVE_WITH_KNOTS('',3,(#10620,#10621,#10622,#10623,#10624,
#10625,#10626,#10627,#10628,#10629,#10630,#10631,#10632,#10633,#10634,#10635,
#10636,#10637),.UNSPECIFIED.,.F.,.F.,(4,2,2,2,2,2,2,2,4),(0.377311571006283,
0.471638607292829,0.565965643579376,0.660294392795971,0.754623142012565,
0.84895189122916,0.943280640445755,1.0376076767323,1.13193471301885),
 .UNSPECIFIED.);
#381=B_SPLINE_CURVE_WITH_KNOTS('',3,(#10639,#10640,#10641,#10642,#10643,
#10644,#10645,#10646,#10647,#10648),.UNSPECIFIED.,.F.,.F.,(4,2,2,2,4),(1.13193471301885,
1.22626174930539,1.32058878559194,1.41491753480854,1.50924628402513),
 .UNSPECIFIED.);
#382=B_SPLINE_CURVE_WITH_KNOTS('',3,(#10649,#10650,#10651,#10652,#10653,
#10654,#10655,#10656,#10657,#10658),.UNSPECIFIED.,.F.,.F.,(4,2,2,2,4),(1.50924628402513,
1.60357503324172,1.69790378245832,1.79223081874487,1.88655785503141),
 .UNSPECIFIED.);
#383=B_SPLINE_CURVE_WITH_KNOTS('',3,(#10662,#10663,#10664,#10665,#10666,
#10667,#10668,#10669,#10670,#10671,#10672,#10673,#10674,#10675,#10676,#10677,
#10678,#10679,#10680,#10681,#10682,#10683,#10684,#10685,#10686,#10687,#10688,
#10689,#10690,#10691,#10692,#10693,#10694,#10695),.UNSPECIFIED.,.T.,.F.,
(4,2,2,2,2,2,2,2,2,2,2,2,2,2,2,2,4),(0.,0.0955080856649705,0.191016171329941,
0.286408845249646,0.38180151916935,0.477194193089055,0.572586867008759,
0.66809495267373,0.7636030383387,0.859111124003671,0.954619209668642,1.05001188358835,
1.14540455750805,1.24079723142776,1.33618990534746,1.43169799101243,1.5272060766774),
 .UNSPECIFIED.);
#384=B_SPLINE_CURVE_WITH_KNOTS('',3,(#10698,#10699,#10700,#10701,#10702,
#10703,#10704,#10705,#10706,#10707,#10708,#10709,#10710,#10711,#10712,#10713,
#10714,#10715,#10716,#10717,#10718,#10719,#10720,#10721,#10722,#10723,#10724,
#10725,#10726,#10727,#10728,#10729,#10730,#10731),.UNSPECIFIED.,.T.,.F.,
(4,2,2,2,2,2,2,2,2,2,2,2,2,2,2,2,4),(0.,0.0955080856649706,0.191016171329941,
0.286408845249646,0.381801519169351,0.477194193089055,0.57258686700876,
0.668094952673731,0.763603038338701,0.859111124003672,0.954619209668642,
1.05001188358835,1.14540455750805,1.24079723142776,1.33618990534746,1.43169799101243,
1.5272060766774),.UNSPECIFIED.);
#385=B_SPLINE_CURVE_WITH_KNOTS('',3,(#10736,#10737,#10738,#10739,#10740,
#10741,#10742,#10743,#10744,#10745,#10746,#10747,#10748,#10749,#10750,#10751,
#10752,#10753,#10754,#10755,#10756,#10757,#10758,#10759,#10760,#10761,#10762,
#10763,#10764,#10765,#10766,#10767,#10768,#10769),.UNSPECIFIED.,.T.,.F.,
(4,2,2,2,2,2,2,2,2,2,2,2,2,2,2,2,4),(0.,0.0955080856649705,0.191016171329941,
0.286408845249646,0.38180151916935,0.477194193089055,0.572586867008759,
0.66809495267373,0.7636030383387,0.859111124003671,0.954619209668642,1.05001188358835,
1.14540455750805,1.24079723142776,1.33618990534746,1.43169799101243,1.5272060766774),
 .UNSPECIFIED.);
#386=B_SPLINE_CURVE_WITH_KNOTS('',3,(#10772,#10773,#10774,#10775,#10776,
#10777,#10778,#10779,#10780,#10781,#10782,#10783,#10784,#10785,#10786,#10787,
#10788,#10789,#10790,#10791,#10792,#10793,#10794,#10795,#10796,#10797,#10798,
#10799,#10800,#10801,#10802,#10803,#10804,#10805),.UNSPECIFIED.,.T.,.F.,
(4,2,2,2,2,2,2,2,2,2,2,2,2,2,2,2,4),(0.,0.0955080856649706,0.191016171329941,
0.286408845249646,0.381801519169351,0.477194193089055,0.57258686700876,
0.668094952673731,0.763603038338701,0.859111124003672,0.954619209668642,
1.05001188358835,1.14540455750805,1.24079723142776,1.33618990534746,1.43169799101243,
1.5272060766774),.UNSPECIFIED.);
#387=B_SPLINE_CURVE_WITH_KNOTS('',3,(#11236,#11237,#11238,#11239,#11240,
#11241,#11242,#11243,#11244,#11245),.UNSPECIFIED.,.F.,.F.,(4,2,2,2,4),(0.847831445683411,
0.878274576930949,0.958092875386315,1.03791117384168,1.06835430508922),
 .UNSPECIFIED.);
#388=B_SPLINE_CURVE_WITH_KNOTS('',3,(#11251,#11252,#11253,#11254,#11255,
#11256,#11257,#11258,#11259,#11260,#11261,#11262,#11263,#11264,#11265,#11266,
#11267,#11268),.UNSPECIFIED.,.F.,.F.,(4,2,2,2,2,2,2,2,4),(0.,0.0792165807733633,
0.158433161546727,0.237648697074571,0.316864232602415,0.396079768130259,
0.475295303658103,0.554511884431466,0.63372846520483),.UNSPECIFIED.);
#389=B_SPLINE_CURVE_WITH_KNOTS('',3,(#11269,#11270,#11271,#11272,#11273,
#11274,#11275,#11276,#11277,#11278,#11279,#11280,#11281,#11282,#11283,#11284,
#11285,#11286),.UNSPECIFIED.,.F.,.F.,(4,2,2,2,2,2,2,2,4),(0.63372846520483,
0.712945045978193,0.792161626751556,0.8713771622794,0.950592697807245,1.02980823333509,
1.10902376886293,1.1882403496363,1.26745693040966),.UNSPECIFIED.);
#390=B_SPLINE_CURVE_WITH_KNOTS('',3,(#11289,#11290,#11291,#11292,#11293,
#11294,#11295,#11296,#11297,#11298),.UNSPECIFIED.,.F.,.F.,(4,2,2,2,4),(0.209102862092535,
0.239545993340072,0.319364291795438,0.399182590250804,0.429625721498342),
 .UNSPECIFIED.);
#391=SPHERICAL_SURFACE('',#7045,2.35);
#392=SPHERICAL_SURFACE('',#7083,2.35);
#393=CONICAL_SURFACE('',#7002,0.4,0.785398163397448);
#394=CONICAL_SURFACE('',#7006,0.41,0.785398163397448);
#395=CONICAL_SURFACE('',#7010,0.26,0.463647609000806);
#396=CONICAL_SURFACE('',#7026,0.475,0.785398163397449);
#397=CONICAL_SURFACE('',#7030,0.485,0.785398163397448);
#398=CONICAL_SURFACE('',#7034,0.31,0.463647609000806);
#399=CONICAL_SURFACE('',#7110,0.625,0.785398163397448);
#400=CONICAL_SURFACE('',#7114,0.635,0.785398163397449);
#401=CONICAL_SURFACE('',#7118,0.41,0.463647609000806);
#402=CONICAL_SURFACE('',#7122,0.36,0.785398163397448);
#403=CONICAL_SURFACE('',#7143,0.734027674973257,1.0471975511966);
#404=CONICAL_SURFACE('',#7145,0.734027674973257,1.0471975511966);
#405=CONICAL_SURFACE('',#7354,0.235,0.785398163397448);
#406=CONICAL_SURFACE('',#7358,0.2125,0.785398163397448);
#407=ORIENTED_CLOSED_SHELL('',*,#6341,.F.);
#408=ORIENTED_CLOSED_SHELL('',*,#6343,.F.);
#409=ORIENTED_CLOSED_SHELL('',*,#6349,.F.);
#410=BREP_WITH_VOIDS('Body1',#6342,(#407));
#411=BREP_WITH_VOIDS('Body1',#6344,(#408));
#412=BREP_WITH_VOIDS('Body1',#6348,(#409));
#413=ELLIPSE('',#6979,0.299389011154384,0.2117);
#414=ELLIPSE('',#6983,0.299389011154384,0.2117);
#415=SHAPE_REPRESENTATION_RELATIONSHIP('SRR','None',#11723,#447);
#416=SHAPE_REPRESENTATION_RELATIONSHIP('SRR','None',#11724,#448);
#417=SHAPE_REPRESENTATION_RELATIONSHIP('SRR','None',#11725,#449);
#418=SHAPE_REPRESENTATION_RELATIONSHIP('SRR','None',#11726,#450);
#419=SHAPE_REPRESENTATION_RELATIONSHIP('SRR','None',#11727,#451);
#420=SHAPE_REPRESENTATION_RELATIONSHIP('SRR','None',#11728,#452);
#421=SHAPE_REPRESENTATION_RELATIONSHIP('SRR','None',#11729,#453);
#422=SHAPE_REPRESENTATION_RELATIONSHIP('SRR','None',#11730,#454);
#423=SHAPE_REPRESENTATION_RELATIONSHIP('SRR','None',#11731,#455);
#424=SHAPE_REPRESENTATION_RELATIONSHIP('SRR','None',#11732,#456);
#425=SHAPE_REPRESENTATION_RELATIONSHIP('SRR','None',#11733,#457);
#426=SHAPE_REPRESENTATION_RELATIONSHIP('SRR','None',#11734,#458);
#427=SHAPE_REPRESENTATION_RELATIONSHIP('SRR','None',#11735,#459);
#428=SHAPE_REPRESENTATION_RELATIONSHIP('SRR','None',#11736,#460);
#429=SHAPE_REPRESENTATION_RELATIONSHIP('SRR','None',#11737,#461);
#430=SHAPE_REPRESENTATION_RELATIONSHIP('SRR','None',#11738,#462);
#431=SHAPE_REPRESENTATION_RELATIONSHIP('SRR','None',#11739,#463);
#432=SHAPE_REPRESENTATION_RELATIONSHIP('SRR','None',#11740,#464);
#433=SHAPE_REPRESENTATION_RELATIONSHIP('SRR','None',#11741,#465);
#434=SHAPE_REPRESENTATION_RELATIONSHIP('SRR','None',#11743,#466);
#435=SHAPE_REPRESENTATION_RELATIONSHIP('SRR','None',#11744,#467);
#436=SHAPE_REPRESENTATION_RELATIONSHIP('SRR','None',#11745,#468);
#437=SHAPE_REPRESENTATION_RELATIONSHIP('SRR','None',#11746,#469);
#438=SHAPE_REPRESENTATION_RELATIONSHIP('SRR','None',#11747,#470);
#439=SHAPE_REPRESENTATION_RELATIONSHIP('SRR','None',#11749,#471);
#440=SHAPE_REPRESENTATION_RELATIONSHIP('SRR','None',#11750,#472);
#441=SHAPE_REPRESENTATION_RELATIONSHIP('SRR','None',#11751,#473);
#442=SHAPE_REPRESENTATION_RELATIONSHIP('SRR','None',#11752,#474);
#443=SHAPE_REPRESENTATION_RELATIONSHIP('SRR','None',#11753,#475);
#444=SHAPE_REPRESENTATION_RELATIONSHIP('SRR','None',#11754,#476);
#445=SHAPE_REPRESENTATION_RELATIONSHIP('SRR','None',#11755,#477);
#446=SHAPE_REPRESENTATION_RELATIONSHIP('SRR','None',#11756,#478);
#447=ADVANCED_BREP_SHAPE_REPRESENTATION('',(#512),#11525);
#448=ADVANCED_BREP_SHAPE_REPRESENTATION('',(#513),#11526);
#449=ADVANCED_BREP_SHAPE_REPRESENTATION('',(#514),#11527);
#450=ADVANCED_BREP_SHAPE_REPRESENTATION('',(#515),#11528);
#451=ADVANCED_BREP_SHAPE_REPRESENTATION('',(#516),#11529);
#452=ADVANCED_BREP_SHAPE_REPRESENTATION('',(#517),#11530);
#453=ADVANCED_BREP_SHAPE_REPRESENTATION('',(#518),#11531);
#454=ADVANCED_BREP_SHAPE_REPRESENTATION('',(#519),#11532);
#455=ADVANCED_BREP_SHAPE_REPRESENTATION('',(#520),#11533);
#456=ADVANCED_BREP_SHAPE_REPRESENTATION('',(#521),#11534);
#457=ADVANCED_BREP_SHAPE_REPRESENTATION('',(#522),#11535);
#458=ADVANCED_BREP_SHAPE_REPRESENTATION('',(#523),#11536);
#459=ADVANCED_BREP_SHAPE_REPRESENTATION('',(#524),#11537);
#460=ADVANCED_BREP_SHAPE_REPRESENTATION('',(#525),#11538);
#461=ADVANCED_BREP_SHAPE_REPRESENTATION('',(#526),#11539);
#462=ADVANCED_BREP_SHAPE_REPRESENTATION('',(#527),#11540);
#463=ADVANCED_BREP_SHAPE_REPRESENTATION('',(#528),#11541);
#464=ADVANCED_BREP_SHAPE_REPRESENTATION('',(#410),#11542);
#465=ADVANCED_BREP_SHAPE_REPRESENTATION('',(#411),#11543);
#466=ADVANCED_BREP_SHAPE_REPRESENTATION('',(#529),#11545);
#467=ADVANCED_BREP_SHAPE_REPRESENTATION('',(#530,#531),#11546);
#468=ADVANCED_BREP_SHAPE_REPRESENTATION('',(#412),#11547);
#469=ADVANCED_BREP_SHAPE_REPRESENTATION('',(#532),#11548);
#470=ADVANCED_BREP_SHAPE_REPRESENTATION('',(#533),#11549);
#471=ADVANCED_BREP_SHAPE_REPRESENTATION('',(#534),#11551);
#472=ADVANCED_BREP_SHAPE_REPRESENTATION('',(#535),#11552);
#473=ADVANCED_BREP_SHAPE_REPRESENTATION('',(#536),#11553);
#474=ADVANCED_BREP_SHAPE_REPRESENTATION('',(#537),#11554);
#475=ADVANCED_BREP_SHAPE_REPRESENTATION('',(#538),#11555);
#476=ADVANCED_BREP_SHAPE_REPRESENTATION('',(#539),#11556);
#477=ADVANCED_BREP_SHAPE_REPRESENTATION('',(#540),#11557);
#478=ADVANCED_BREP_SHAPE_REPRESENTATION('',(#541),#11558);
#479=STYLED_ITEM('',(#11946),#512);
#480=STYLED_ITEM('',(#11960),#513);
#481=STYLED_ITEM('',(#11960),#514);
#482=STYLED_ITEM('',(#11960),#515);
#483=STYLED_ITEM('',(#11960),#516);
#484=STYLED_ITEM('',(#11953),#517);
#485=STYLED_ITEM('',(#11981),#518);
#486=STYLED_ITEM('',(#11981),#519);
#487=STYLED_ITEM('',(#11981),#520);
#488=STYLED_ITEM('',(#11981),#521);
#489=STYLED_ITEM('',(#11953),#522);
#490=STYLED_ITEM('',(#11981),#523);
#491=STYLED_ITEM('',(#11981),#524);
#492=STYLED_ITEM('',(#11981),#525);
#493=STYLED_ITEM('',(#11981),#526);
#494=STYLED_ITEM('',(#11981),#527);
#495=STYLED_ITEM('',(#11974),#528);
#496=STYLED_ITEM('',(#11974),#410);
#497=STYLED_ITEM('',(#11974),#411);
#498=STYLED_ITEM('',(#11946),#529);
#499=STYLED_ITEM('',(#11967),#530);
#500=STYLED_ITEM('',(#11967),#531);
#501=STYLED_ITEM('',(#11974),#412);
#502=STYLED_ITEM('',(#11974),#532);
#503=STYLED_ITEM('',(#11974),#533);
#504=STYLED_ITEM('',(#11967),#534);
#505=STYLED_ITEM('',(#11953),#535);
#506=STYLED_ITEM('',(#11960),#536);
#507=STYLED_ITEM('',(#11974),#537);
#508=STYLED_ITEM('',(#11974),#538);
#509=STYLED_ITEM('',(#11953),#539);
#510=STYLED_ITEM('',(#11967),#540);
#511=STYLED_ITEM('',(#11974),#541);
#512=MANIFOLD_SOLID_BREP('Body1',#6324);
#513=MANIFOLD_SOLID_BREP('Body1',#6325);
#514=MANIFOLD_SOLID_BREP('Body1',#6326);
#515=MANIFOLD_SOLID_BREP('Body1',#6327);
#516=MANIFOLD_SOLID_BREP('Body1',#6328);
#517=MANIFOLD_SOLID_BREP('Body1',#6329);
#518=MANIFOLD_SOLID_BREP('Body1',#6330);
#519=MANIFOLD_SOLID_BREP('Body1',#6331);
#520=MANIFOLD_SOLID_BREP('Body1',#6332);
#521=MANIFOLD_SOLID_BREP('Body1',#6333);
#522=MANIFOLD_SOLID_BREP('Body1',#6334);
#523=MANIFOLD_SOLID_BREP('Body1',#6335);
#524=MANIFOLD_SOLID_BREP('Body1',#6336);
#525=MANIFOLD_SOLID_BREP('Body1',#6337);
#526=MANIFOLD_SOLID_BREP('Body1',#6338);
#527=MANIFOLD_SOLID_BREP('Body1',#6339);
#528=MANIFOLD_SOLID_BREP('Body1',#6340);
#529=MANIFOLD_SOLID_BREP('Body1',#6345);
#530=MANIFOLD_SOLID_BREP('Body1',#6346);
#531=MANIFOLD_SOLID_BREP('Body2',#6347);
#532=MANIFOLD_SOLID_BREP('Body1',#6350);
#533=MANIFOLD_SOLID_BREP('Body1',#6351);
#534=MANIFOLD_SOLID_BREP('Body1',#6352);
#535=MANIFOLD_SOLID_BREP('Body1',#6353);
#536=MANIFOLD_SOLID_BREP('Body1',#6354);
#537=MANIFOLD_SOLID_BREP('Body1',#6355);
#538=MANIFOLD_SOLID_BREP('Body1',#6356);
#539=MANIFOLD_SOLID_BREP('Body1',#6357);
#540=MANIFOLD_SOLID_BREP('Body1',#6358);
#541=MANIFOLD_SOLID_BREP('Body1',#6359);
#542=FACE_BOUND('',#1278,.T.);
#543=FACE_BOUND('',#1279,.T.);
#544=FACE_BOUND('',#1280,.T.);
#545=FACE_BOUND('',#1281,.T.);
#546=FACE_BOUND('',#1282,.T.);
#547=FACE_BOUND('',#1283,.T.);
#548=FACE_BOUND('',#1284,.T.);
#549=FACE_BOUND('',#1285,.T.);
#550=FACE_BOUND('',#1286,.T.);
#551=FACE_BOUND('',#1287,.T.);
#552=FACE_BOUND('',#1288,.T.);
#553=FACE_BOUND('',#1289,.T.);
#554=FACE_BOUND('',#1291,.T.);
#555=FACE_BOUND('',#1292,.T.);
#556=FACE_BOUND('',#1293,.T.);
#557=FACE_BOUND('',#1294,.T.);
#558=FACE_BOUND('',#1295,.T.);
#559=FACE_BOUND('',#1296,.T.);
#560=FACE_BOUND('',#1297,.T.);
#561=FACE_BOUND('',#1298,.T.);
#562=FACE_BOUND('',#1299,.T.);
#563=FACE_BOUND('',#1300,.T.);
#564=FACE_BOUND('',#1301,.T.);
#565=FACE_BOUND('',#1302,.T.);
#566=FACE_BOUND('',#1335,.T.);
#567=FACE_BOUND('',#1336,.T.);
#568=FACE_BOUND('',#1339,.T.);
#569=FACE_BOUND('',#1340,.T.);
#570=FACE_BOUND('',#1341,.T.);
#571=FACE_BOUND('',#1342,.T.);
#572=FACE_BOUND('',#1343,.T.);
#573=FACE_BOUND('',#1347,.T.);
#574=FACE_BOUND('',#1348,.T.);
#575=FACE_BOUND('',#1349,.T.);
#576=FACE_BOUND('',#1350,.T.);
#577=FACE_BOUND('',#1351,.T.);
#578=FACE_BOUND('',#1354,.T.);
#579=FACE_BOUND('',#1355,.T.);
#580=FACE_BOUND('',#1359,.T.);
#581=FACE_BOUND('',#1361,.T.);
#582=FACE_BOUND('',#1365,.T.);
#583=FACE_BOUND('',#1367,.T.);
#584=FACE_BOUND('',#1371,.T.);
#585=FACE_BOUND('',#1373,.T.);
#586=FACE_BOUND('',#1377,.T.);
#587=FACE_BOUND('',#1379,.T.);
#588=FACE_BOUND('',#1388,.T.);
#589=FACE_BOUND('',#1389,.T.);
#590=FACE_BOUND('',#1392,.T.);
#591=FACE_BOUND('',#1393,.T.);
#592=FACE_BOUND('',#1394,.T.);
#593=FACE_BOUND('',#1395,.T.);
#594=FACE_BOUND('',#1396,.T.);
#595=FACE_BOUND('',#1400,.T.);
#596=FACE_BOUND('',#1401,.T.);
#597=FACE_BOUND('',#1402,.T.);
#598=FACE_BOUND('',#1403,.T.);
#599=FACE_BOUND('',#1404,.T.);
#600=FACE_BOUND('',#1407,.T.);
#601=FACE_BOUND('',#1408,.T.);
#602=FACE_BOUND('',#1412,.T.);
#603=FACE_BOUND('',#1414,.T.);
#604=FACE_BOUND('',#1418,.T.);
#605=FACE_BOUND('',#1420,.T.);
#606=FACE_BOUND('',#1424,.T.);
#607=FACE_BOUND('',#1426,.T.);
#608=FACE_BOUND('',#1430,.T.);
#609=FACE_BOUND('',#1432,.T.);
#610=FACE_BOUND('',#1479,.T.);
#611=FACE_BOUND('',#1481,.T.);
#612=FACE_BOUND('',#1485,.T.);
#613=FACE_BOUND('',#1511,.T.);
#614=FACE_BOUND('',#1528,.T.);
#615=FACE_BOUND('',#1534,.T.);
#616=FACE_BOUND('',#1535,.T.);
#617=FACE_BOUND('',#1539,.T.);
#618=FACE_BOUND('',#1541,.T.);
#619=FACE_BOUND('',#1555,.T.);
#620=FACE_BOUND('',#1556,.T.);
#621=FACE_BOUND('',#1557,.T.);
#622=FACE_BOUND('',#1558,.T.);
#623=FACE_BOUND('',#1559,.T.);
#624=FACE_BOUND('',#1561,.T.);
#625=FACE_BOUND('',#1562,.T.);
#626=FACE_BOUND('',#1563,.T.);
#627=FACE_BOUND('',#1564,.T.);
#628=FACE_BOUND('',#1565,.T.);
#629=FACE_BOUND('',#1568,.T.);
#630=FACE_BOUND('',#1570,.T.);
#631=FACE_BOUND('',#1571,.T.);
#632=FACE_BOUND('',#1573,.T.);
#633=FACE_BOUND('',#1577,.T.);
#634=FACE_BOUND('',#1578,.T.);
#635=FACE_BOUND('',#1579,.T.);
#636=FACE_BOUND('',#1580,.T.);
#637=FACE_BOUND('',#1581,.T.);
#638=FACE_BOUND('',#1582,.T.);
#639=FACE_BOUND('',#1588,.T.);
#640=FACE_BOUND('',#1590,.T.);
#641=FACE_BOUND('',#1593,.T.);
#642=FACE_BOUND('',#1595,.T.);
#643=FACE_BOUND('',#1596,.T.);
#644=FACE_BOUND('',#1597,.T.);
#645=FACE_BOUND('',#1598,.T.);
#646=FACE_BOUND('',#1599,.T.);
#647=FACE_BOUND('',#1600,.T.);
#648=FACE_BOUND('',#1606,.T.);
#649=FACE_BOUND('',#1622,.T.);
#650=FACE_BOUND('',#1624,.T.);
#651=FACE_BOUND('',#1635,.T.);
#652=FACE_BOUND('',#1637,.T.);
#653=FACE_BOUND('',#1644,.T.);
#654=FACE_BOUND('',#1646,.T.);
#655=FACE_BOUND('',#1650,.T.);
#656=FACE_BOUND('',#1656,.T.);
#657=FACE_BOUND('',#1658,.T.);
#658=FACE_BOUND('',#1662,.T.);
#659=FACE_BOUND('',#1664,.T.);
#660=FACE_BOUND('',#1673,.T.);
#661=FACE_BOUND('',#1675,.T.);
#662=FACE_BOUND('',#1684,.T.);
#663=FACE_BOUND('',#1686,.T.);
#664=FACE_BOUND('',#1694,.T.);
#665=FACE_BOUND('',#1696,.T.);
#666=FACE_BOUND('',#1702,.T.);
#667=FACE_BOUND('',#1703,.T.);
#668=FACE_BOUND('',#1704,.T.);
#669=FACE_BOUND('',#1705,.T.);
#670=FACE_BOUND('',#1706,.T.);
#671=FACE_BOUND('',#1708,.T.);
#672=FACE_BOUND('',#1709,.T.);
#673=FACE_BOUND('',#1710,.T.);
#674=FACE_BOUND('',#1711,.T.);
#675=FACE_BOUND('',#1712,.T.);
#676=FACE_BOUND('',#1715,.T.);
#677=FACE_BOUND('',#1718,.T.);
#678=FACE_BOUND('',#1737,.T.);
#679=PLANE('',#6752);
#680=PLANE('',#6753);
#681=PLANE('',#6754);
#682=PLANE('',#6755);
#683=PLANE('',#6756);
#684=PLANE('',#6757);
#685=PLANE('',#6759);
#686=PLANE('',#6760);
#687=PLANE('',#6761);
#688=PLANE('',#6762);
#689=PLANE('',#6763);
#690=PLANE('',#6764);
#691=PLANE('',#6766);
#692=PLANE('',#6767);
#693=PLANE('',#6768);
#694=PLANE('',#6769);
#695=PLANE('',#6770);
#696=PLANE('',#6771);
#697=PLANE('',#6773);
#698=PLANE('',#6774);
#699=PLANE('',#6775);
#700=PLANE('',#6776);
#701=PLANE('',#6777);
#702=PLANE('',#6778);
#703=PLANE('',#6780);
#704=PLANE('',#6781);
#705=PLANE('',#6782);
#706=PLANE('',#6783);
#707=PLANE('',#6784);
#708=PLANE('',#6785);
#709=PLANE('',#6808);
#710=PLANE('',#6809);
#711=PLANE('',#6810);
#712=PLANE('',#6811);
#713=PLANE('',#6812);
#714=PLANE('',#6813);
#715=PLANE('',#6814);
#716=PLANE('',#6815);
#717=PLANE('',#6823);
#718=PLANE('',#6824);
#719=PLANE('',#6832);
#720=PLANE('',#6833);
#721=PLANE('',#6841);
#722=PLANE('',#6842);
#723=PLANE('',#6850);
#724=PLANE('',#6851);
#725=PLANE('',#6874);
#726=PLANE('',#6875);
#727=PLANE('',#6876);
#728=PLANE('',#6877);
#729=PLANE('',#6878);
#730=PLANE('',#6879);
#731=PLANE('',#6880);
#732=PLANE('',#6881);
#733=PLANE('',#6889);
#734=PLANE('',#6890);
#735=PLANE('',#6898);
#736=PLANE('',#6899);
#737=PLANE('',#6907);
#738=PLANE('',#6908);
#739=PLANE('',#6916);
#740=PLANE('',#6917);
#741=PLANE('',#6919);
#742=PLANE('',#6920);
#743=PLANE('',#6921);
#744=PLANE('',#6922);
#745=PLANE('',#6923);
#746=PLANE('',#6924);
#747=PLANE('',#6925);
#748=PLANE('',#6926);
#749=PLANE('',#6927);
#750=PLANE('',#6928);
#751=PLANE('',#6929);
#752=PLANE('',#6930);
#753=PLANE('',#6931);
#754=PLANE('',#6932);
#755=PLANE('',#6933);
#756=PLANE('',#6934);
#757=PLANE('',#6935);
#758=PLANE('',#6936);
#759=PLANE('',#6937);
#760=PLANE('',#6938);
#761=PLANE('',#6939);
#762=PLANE('',#6940);
#763=PLANE('',#6941);
#764=PLANE('',#6942);
#765=PLANE('',#6943);
#766=PLANE('',#6944);
#767=PLANE('',#6945);
#768=PLANE('',#6946);
#769=PLANE('',#6947);
#770=PLANE('',#6948);
#771=PLANE('',#6949);
#772=PLANE('',#6950);
#773=PLANE('',#6951);
#774=PLANE('',#6952);
#775=PLANE('',#6953);
#776=PLANE('',#6954);
#777=PLANE('',#6958);
#778=PLANE('',#6959);
#779=PLANE('',#6960);
#780=PLANE('',#6961);
#781=PLANE('',#6962);
#782=PLANE('',#6963);
#783=PLANE('',#6964);
#784=PLANE('',#6965);
#785=PLANE('',#6966);
#786=PLANE('',#6967);
#787=PLANE('',#6969);
#788=PLANE('',#6970);
#789=PLANE('',#6971);
#790=PLANE('',#6973);
#791=PLANE('',#6974);
#792=PLANE('',#6975);
#793=PLANE('',#6976);
#794=PLANE('',#6977);
#795=PLANE('',#6978);
#796=PLANE('',#6985);
#797=PLANE('',#6986);
#798=PLANE('',#6987);
#799=PLANE('',#6988);
#800=PLANE('',#6990);
#801=PLANE('',#6991);
#802=PLANE('',#6992);
#803=PLANE('',#6993);
#804=PLANE('',#6994);
#805=PLANE('',#6995);
#806=PLANE('',#6996);
#807=PLANE('',#6997);
#808=PLANE('',#6998);
#809=PLANE('',#7000);
#810=PLANE('',#7008);
#811=PLANE('',#7014);
#812=PLANE('',#7015);
#813=PLANE('',#7016);
#814=PLANE('',#7017);
#815=PLANE('',#7018);
#816=PLANE('',#7019);
#817=PLANE('',#7020);
#818=PLANE('',#7021);
#819=PLANE('',#7022);
#820=PLANE('',#7024);
#821=PLANE('',#7032);
#822=PLANE('',#7053);
#823=PLANE('',#7054);
#824=PLANE('',#7067);
#825=PLANE('',#7068);
#826=PLANE('',#7069);
#827=PLANE('',#7070);
#828=PLANE('',#7071);
#829=PLANE('',#7072);
#830=PLANE('',#7073);
#831=PLANE('',#7074);
#832=PLANE('',#7075);
#833=PLANE('',#7076);
#834=PLANE('',#7081);
#835=PLANE('',#7086);
#836=PLANE('',#7096);
#837=PLANE('',#7098);
#838=PLANE('',#7102);
#839=PLANE('',#7108);
#840=PLANE('',#7116);
#841=PLANE('',#7124);
#842=PLANE('',#7125);
#843=PLANE('',#7126);
#844=PLANE('',#7127);
#845=PLANE('',#7128);
#846=PLANE('',#7129);
#847=PLANE('',#7130);
#848=PLANE('',#7131);
#849=PLANE('',#7132);
#850=PLANE('',#7140);
#851=PLANE('',#7141);
#852=PLANE('',#7147);
#853=PLANE('',#7148);
#854=PLANE('',#7149);
#855=PLANE('',#7153);
#856=PLANE('',#7154);
#857=PLANE('',#7155);
#858=PLANE('',#7156);
#859=PLANE('',#7157);
#860=PLANE('',#7233);
#861=PLANE('',#7234);
#862=PLANE('',#7236);
#863=PLANE('',#7237);
#864=PLANE('',#7238);
#865=PLANE('',#7240);
#866=PLANE('',#7243);
#867=PLANE('',#7251);
#868=PLANE('',#7252);
#869=PLANE('',#7260);
#870=PLANE('',#7261);
#871=PLANE('',#7269);
#872=PLANE('',#7270);
#873=PLANE('',#7275);
#874=PLANE('',#7276);
#875=PLANE('',#7277);
#876=PLANE('',#7278);
#877=PLANE('',#7279);
#878=PLANE('',#7280);
#879=PLANE('',#7281);
#880=PLANE('',#7282);
#881=PLANE('',#7287);
#882=PLANE('',#7288);
#883=PLANE('',#7289);
#884=PLANE('',#7290);
#885=PLANE('',#7291);
#886=PLANE('',#7292);
#887=PLANE('',#7293);
#888=PLANE('',#7294);
#889=PLANE('',#7296);
#890=PLANE('',#7301);
#891=PLANE('',#7302);
#892=PLANE('',#7303);
#893=PLANE('',#7304);
#894=PLANE('',#7305);
#895=PLANE('',#7322);
#896=PLANE('',#7325);
#897=PLANE('',#7332);
#898=PLANE('',#7334);
#899=PLANE('',#7335);
#900=PLANE('',#7336);
#901=PLANE('',#7337);
#902=PLANE('',#7338);
#903=PLANE('',#7339);
#904=PLANE('',#7340);
#905=PLANE('',#7341);
#906=PLANE('',#7342);
#907=PLANE('',#7343);
#908=PLANE('',#7345);
#909=PLANE('',#7346);
#910=PLANE('',#7347);
#911=PLANE('',#7348);
#912=PLANE('',#7349);
#913=PLANE('',#7350);
#914=PLANE('',#7351);
#915=PLANE('',#7352);
#916=PLANE('',#7360);
#917=FACE_OUTER_BOUND('',#1261,.T.);
#918=FACE_OUTER_BOUND('',#1262,.T.);
#919=FACE_OUTER_BOUND('',#1263,.T.);
#920=FACE_OUTER_BOUND('',#1264,.T.);
#921=FACE_OUTER_BOUND('',#1265,.T.);
#922=FACE_OUTER_BOUND('',#1266,.T.);
#923=FACE_OUTER_BOUND('',#1267,.T.);
#924=FACE_OUTER_BOUND('',#1268,.T.);
#925=FACE_OUTER_BOUND('',#1269,.T.);
#926=FACE_OUTER_BOUND('',#1270,.T.);
#927=FACE_OUTER_BOUND('',#1271,.T.);
#928=FACE_OUTER_BOUND('',#1272,.T.);
#929=FACE_OUTER_BOUND('',#1273,.T.);
#930=FACE_OUTER_BOUND('',#1274,.T.);
#931=FACE_OUTER_BOUND('',#1275,.T.);
#932=FACE_OUTER_BOUND('',#1276,.T.);
#933=FACE_OUTER_BOUND('',#1277,.T.);
#934=FACE_OUTER_BOUND('',#1290,.T.);
#935=FACE_OUTER_BOUND('',#1303,.T.);
#936=FACE_OUTER_BOUND('',#1304,.T.);
#937=FACE_OUTER_BOUND('',#1305,.T.);
#938=FACE_OUTER_BOUND('',#1306,.T.);
#939=FACE_OUTER_BOUND('',#1307,.T.);
#940=FACE_OUTER_BOUND('',#1308,.T.);
#941=FACE_OUTER_BOUND('',#1309,.T.);
#942=FACE_OUTER_BOUND('',#1310,.T.);
#943=FACE_OUTER_BOUND('',#1311,.T.);
#944=FACE_OUTER_BOUND('',#1312,.T.);
#945=FACE_OUTER_BOUND('',#1313,.T.);
#946=FACE_OUTER_BOUND('',#1314,.T.);
#947=FACE_OUTER_BOUND('',#1315,.T.);
#948=FACE_OUTER_BOUND('',#1316,.T.);
#949=FACE_OUTER_BOUND('',#1317,.T.);
#950=FACE_OUTER_BOUND('',#1318,.T.);
#951=FACE_OUTER_BOUND('',#1319,.T.);
#952=FACE_OUTER_BOUND('',#1320,.T.);
#953=FACE_OUTER_BOUND('',#1321,.T.);
#954=FACE_OUTER_BOUND('',#1322,.T.);
#955=FACE_OUTER_BOUND('',#1323,.T.);
#956=FACE_OUTER_BOUND('',#1324,.T.);
#957=FACE_OUTER_BOUND('',#1325,.T.);
#958=FACE_OUTER_BOUND('',#1326,.T.);
#959=FACE_OUTER_BOUND('',#1327,.T.);
#960=FACE_OUTER_BOUND('',#1328,.T.);
#961=FACE_OUTER_BOUND('',#1329,.T.);
#962=FACE_OUTER_BOUND('',#1330,.T.);
#963=FACE_OUTER_BOUND('',#1331,.T.);
#964=FACE_OUTER_BOUND('',#1332,.T.);
#965=FACE_OUTER_BOUND('',#1333,.T.);
#966=FACE_OUTER_BOUND('',#1334,.T.);
#967=FACE_OUTER_BOUND('',#1337,.T.);
#968=FACE_OUTER_BOUND('',#1338,.T.);
#969=FACE_OUTER_BOUND('',#1344,.T.);
#970=FACE_OUTER_BOUND('',#1345,.T.);
#971=FACE_OUTER_BOUND('',#1346,.T.);
#972=FACE_OUTER_BOUND('',#1352,.T.);
#973=FACE_OUTER_BOUND('',#1353,.T.);
#974=FACE_OUTER_BOUND('',#1356,.T.);
#975=FACE_OUTER_BOUND('',#1357,.T.);
#976=FACE_OUTER_BOUND('',#1358,.T.);
#977=FACE_OUTER_BOUND('',#1360,.T.);
#978=FACE_OUTER_BOUND('',#1362,.T.);
#979=FACE_OUTER_BOUND('',#1363,.T.);
#980=FACE_OUTER_BOUND('',#1364,.T.);
#981=FACE_OUTER_BOUND('',#1366,.T.);
#982=FACE_OUTER_BOUND('',#1368,.T.);
#983=FACE_OUTER_BOUND('',#1369,.T.);
#984=FACE_OUTER_BOUND('',#1370,.T.);
#985=FACE_OUTER_BOUND('',#1372,.T.);
#986=FACE_OUTER_BOUND('',#1374,.T.);
#987=FACE_OUTER_BOUND('',#1375,.T.);
#988=FACE_OUTER_BOUND('',#1376,.T.);
#989=FACE_OUTER_BOUND('',#1378,.T.);
#990=FACE_OUTER_BOUND('',#1380,.T.);
#991=FACE_OUTER_BOUND('',#1381,.T.);
#992=FACE_OUTER_BOUND('',#1382,.T.);
#993=FACE_OUTER_BOUND('',#1383,.T.);
#994=FACE_OUTER_BOUND('',#1384,.T.);
#995=FACE_OUTER_BOUND('',#1385,.T.);
#996=FACE_OUTER_BOUND('',#1386,.T.);
#997=FACE_OUTER_BOUND('',#1387,.T.);
#998=FACE_OUTER_BOUND('',#1390,.T.);
#999=FACE_OUTER_BOUND('',#1391,.T.);
#1000=FACE_OUTER_BOUND('',#1397,.T.);
#1001=FACE_OUTER_BOUND('',#1398,.T.);
#1002=FACE_OUTER_BOUND('',#1399,.T.);
#1003=FACE_OUTER_BOUND('',#1405,.T.);
#1004=FACE_OUTER_BOUND('',#1406,.T.);
#1005=FACE_OUTER_BOUND('',#1409,.T.);
#1006=FACE_OUTER_BOUND('',#1410,.T.);
#1007=FACE_OUTER_BOUND('',#1411,.T.);
#1008=FACE_OUTER_BOUND('',#1413,.T.);
#1009=FACE_OUTER_BOUND('',#1415,.T.);
#1010=FACE_OUTER_BOUND('',#1416,.T.);
#1011=FACE_OUTER_BOUND('',#1417,.T.);
#1012=FACE_OUTER_BOUND('',#1419,.T.);
#1013=FACE_OUTER_BOUND('',#1421,.T.);
#1014=FACE_OUTER_BOUND('',#1422,.T.);
#1015=FACE_OUTER_BOUND('',#1423,.T.);
#1016=FACE_OUTER_BOUND('',#1425,.T.);
#1017=FACE_OUTER_BOUND('',#1427,.T.);
#1018=FACE_OUTER_BOUND('',#1428,.T.);
#1019=FACE_OUTER_BOUND('',#1429,.T.);
#1020=FACE_OUTER_BOUND('',#1431,.T.);
#1021=FACE_OUTER_BOUND('',#1433,.T.);
#1022=FACE_OUTER_BOUND('',#1434,.T.);
#1023=FACE_OUTER_BOUND('',#1435,.T.);
#1024=FACE_OUTER_BOUND('',#1436,.T.);
#1025=FACE_OUTER_BOUND('',#1437,.T.);
#1026=FACE_OUTER_BOUND('',#1438,.T.);
#1027=FACE_OUTER_BOUND('',#1439,.T.);
#1028=FACE_OUTER_BOUND('',#1440,.T.);
#1029=FACE_OUTER_BOUND('',#1441,.T.);
#1030=FACE_OUTER_BOUND('',#1442,.T.);
#1031=FACE_OUTER_BOUND('',#1443,.T.);
#1032=FACE_OUTER_BOUND('',#1444,.T.);
#1033=FACE_OUTER_BOUND('',#1445,.T.);
#1034=FACE_OUTER_BOUND('',#1446,.T.);
#1035=FACE_OUTER_BOUND('',#1447,.T.);
#1036=FACE_OUTER_BOUND('',#1448,.T.);
#1037=FACE_OUTER_BOUND('',#1449,.T.);
#1038=FACE_OUTER_BOUND('',#1450,.T.);
#1039=FACE_OUTER_BOUND('',#1451,.T.);
#1040=FACE_OUTER_BOUND('',#1452,.T.);
#1041=FACE_OUTER_BOUND('',#1453,.T.);
#1042=FACE_OUTER_BOUND('',#1454,.T.);
#1043=FACE_OUTER_BOUND('',#1455,.T.);
#1044=FACE_OUTER_BOUND('',#1456,.T.);
#1045=FACE_OUTER_BOUND('',#1457,.T.);
#1046=FACE_OUTER_BOUND('',#1458,.T.);
#1047=FACE_OUTER_BOUND('',#1459,.T.);
#1048=FACE_OUTER_BOUND('',#1460,.T.);
#1049=FACE_OUTER_BOUND('',#1461,.T.);
#1050=FACE_OUTER_BOUND('',#1462,.T.);
#1051=FACE_OUTER_BOUND('',#1463,.T.);
#1052=FACE_OUTER_BOUND('',#1464,.T.);
#1053=FACE_OUTER_BOUND('',#1465,.T.);
#1054=FACE_OUTER_BOUND('',#1466,.T.);
#1055=FACE_OUTER_BOUND('',#1467,.T.);
#1056=FACE_OUTER_BOUND('',#1468,.T.);
#1057=FACE_OUTER_BOUND('',#1469,.T.);
#1058=FACE_OUTER_BOUND('',#1470,.T.);
#1059=FACE_OUTER_BOUND('',#1471,.T.);
#1060=FACE_OUTER_BOUND('',#1472,.T.);
#1061=FACE_OUTER_BOUND('',#1473,.T.);
#1062=FACE_OUTER_BOUND('',#1474,.T.);
#1063=FACE_OUTER_BOUND('',#1475,.T.);
#1064=FACE_OUTER_BOUND('',#1476,.T.);
#1065=FACE_OUTER_BOUND('',#1477,.T.);
#1066=FACE_OUTER_BOUND('',#1478,.T.);
#1067=FACE_OUTER_BOUND('',#1480,.T.);
#1068=FACE_OUTER_BOUND('',#1482,.T.);
#1069=FACE_OUTER_BOUND('',#1483,.T.);
#1070=FACE_OUTER_BOUND('',#1484,.T.);
#1071=FACE_OUTER_BOUND('',#1486,.T.);
#1072=FACE_OUTER_BOUND('',#1487,.T.);
#1073=FACE_OUTER_BOUND('',#1488,.T.);
#1074=FACE_OUTER_BOUND('',#1489,.T.);
#1075=FACE_OUTER_BOUND('',#1490,.T.);
#1076=FACE_OUTER_BOUND('',#1491,.T.);
#1077=FACE_OUTER_BOUND('',#1492,.T.);
#1078=FACE_OUTER_BOUND('',#1493,.T.);
#1079=FACE_OUTER_BOUND('',#1494,.T.);
#1080=FACE_OUTER_BOUND('',#1495,.T.);
#1081=FACE_OUTER_BOUND('',#1496,.T.);
#1082=FACE_OUTER_BOUND('',#1497,.T.);
#1083=FACE_OUTER_BOUND('',#1498,.T.);
#1084=FACE_OUTER_BOUND('',#1499,.T.);
#1085=FACE_OUTER_BOUND('',#1500,.T.);
#1086=FACE_OUTER_BOUND('',#1501,.T.);
#1087=FACE_OUTER_BOUND('',#1502,.T.);
#1088=FACE_OUTER_BOUND('',#1503,.T.);
#1089=FACE_OUTER_BOUND('',#1504,.T.);
#1090=FACE_OUTER_BOUND('',#1505,.T.);
#1091=FACE_OUTER_BOUND('',#1506,.T.);
#1092=FACE_OUTER_BOUND('',#1507,.T.);
#1093=FACE_OUTER_BOUND('',#1508,.T.);
#1094=FACE_OUTER_BOUND('',#1509,.T.);
#1095=FACE_OUTER_BOUND('',#1510,.T.);
#1096=FACE_OUTER_BOUND('',#1512,.T.);
#1097=FACE_OUTER_BOUND('',#1513,.T.);
#1098=FACE_OUTER_BOUND('',#1514,.T.);
#1099=FACE_OUTER_BOUND('',#1515,.T.);
#1100=FACE_OUTER_BOUND('',#1516,.T.);
#1101=FACE_OUTER_BOUND('',#1517,.T.);
#1102=FACE_OUTER_BOUND('',#1518,.T.);
#1103=FACE_OUTER_BOUND('',#1519,.T.);
#1104=FACE_OUTER_BOUND('',#1520,.T.);
#1105=FACE_OUTER_BOUND('',#1521,.T.);
#1106=FACE_OUTER_BOUND('',#1522,.T.);
#1107=FACE_OUTER_BOUND('',#1523,.T.);
#1108=FACE_OUTER_BOUND('',#1524,.T.);
#1109=FACE_OUTER_BOUND('',#1525,.T.);
#1110=FACE_OUTER_BOUND('',#1526,.T.);
#1111=FACE_OUTER_BOUND('',#1527,.T.);
#1112=FACE_OUTER_BOUND('',#1529,.T.);
#1113=FACE_OUTER_BOUND('',#1530,.T.);
#1114=FACE_OUTER_BOUND('',#1531,.T.);
#1115=FACE_OUTER_BOUND('',#1532,.T.);
#1116=FACE_OUTER_BOUND('',#1533,.T.);
#1117=FACE_OUTER_BOUND('',#1536,.T.);
#1118=FACE_OUTER_BOUND('',#1537,.T.);
#1119=FACE_OUTER_BOUND('',#1538,.T.);
#1120=FACE_OUTER_BOUND('',#1540,.T.);
#1121=FACE_OUTER_BOUND('',#1542,.T.);
#1122=FACE_OUTER_BOUND('',#1543,.T.);
#1123=FACE_OUTER_BOUND('',#1544,.T.);
#1124=FACE_OUTER_BOUND('',#1545,.T.);
#1125=FACE_OUTER_BOUND('',#1546,.T.);
#1126=FACE_OUTER_BOUND('',#1547,.T.);
#1127=FACE_OUTER_BOUND('',#1548,.T.);
#1128=FACE_OUTER_BOUND('',#1549,.T.);
#1129=FACE_OUTER_BOUND('',#1550,.T.);
#1130=FACE_OUTER_BOUND('',#1551,.T.);
#1131=FACE_OUTER_BOUND('',#1552,.T.);
#1132=FACE_OUTER_BOUND('',#1553,.T.);
#1133=FACE_OUTER_BOUND('',#1554,.T.);
#1134=FACE_OUTER_BOUND('',#1560,.T.);
#1135=FACE_OUTER_BOUND('',#1566,.T.);
#1136=FACE_OUTER_BOUND('',#1567,.T.);
#1137=FACE_OUTER_BOUND('',#1569,.T.);
#1138=FACE_OUTER_BOUND('',#1572,.T.);
#1139=FACE_OUTER_BOUND('',#1574,.T.);
#1140=FACE_OUTER_BOUND('',#1575,.T.);
#1141=FACE_OUTER_BOUND('',#1576,.T.);
#1142=FACE_OUTER_BOUND('',#1583,.T.);
#1143=FACE_OUTER_BOUND('',#1584,.T.);
#1144=FACE_OUTER_BOUND('',#1585,.T.);
#1145=FACE_OUTER_BOUND('',#1586,.T.);
#1146=FACE_OUTER_BOUND('',#1587,.T.);
#1147=FACE_OUTER_BOUND('',#1589,.T.);
#1148=FACE_OUTER_BOUND('',#1591,.T.);
#1149=FACE_OUTER_BOUND('',#1592,.T.);
#1150=FACE_OUTER_BOUND('',#1594,.T.);
#1151=FACE_OUTER_BOUND('',#1601,.T.);
#1152=FACE_OUTER_BOUND('',#1602,.T.);
#1153=FACE_OUTER_BOUND('',#1603,.T.);
#1154=FACE_OUTER_BOUND('',#1604,.T.);
#1155=FACE_OUTER_BOUND('',#1605,.T.);
#1156=FACE_OUTER_BOUND('',#1607,.T.);
#1157=FACE_OUTER_BOUND('',#1608,.T.);
#1158=FACE_OUTER_BOUND('',#1609,.T.);
#1159=FACE_OUTER_BOUND('',#1610,.T.);
#1160=FACE_OUTER_BOUND('',#1611,.T.);
#1161=FACE_OUTER_BOUND('',#1612,.T.);
#1162=FACE_OUTER_BOUND('',#1613,.T.);
#1163=FACE_OUTER_BOUND('',#1614,.T.);
#1164=FACE_OUTER_BOUND('',#1615,.T.);
#1165=FACE_OUTER_BOUND('',#1616,.T.);
#1166=FACE_OUTER_BOUND('',#1617,.T.);
#1167=FACE_OUTER_BOUND('',#1618,.T.);
#1168=FACE_OUTER_BOUND('',#1619,.T.);
#1169=FACE_OUTER_BOUND('',#1620,.T.);
#1170=FACE_OUTER_BOUND('',#1621,.T.);
#1171=FACE_OUTER_BOUND('',#1623,.T.);
#1172=FACE_OUTER_BOUND('',#1625,.T.);
#1173=FACE_OUTER_BOUND('',#1626,.T.);
#1174=FACE_OUTER_BOUND('',#1627,.T.);
#1175=FACE_OUTER_BOUND('',#1628,.T.);
#1176=FACE_OUTER_BOUND('',#1629,.T.);
#1177=FACE_OUTER_BOUND('',#1630,.T.);
#1178=FACE_OUTER_BOUND('',#1631,.T.);
#1179=FACE_OUTER_BOUND('',#1632,.T.);
#1180=FACE_OUTER_BOUND('',#1633,.T.);
#1181=FACE_OUTER_BOUND('',#1634,.T.);
#1182=FACE_OUTER_BOUND('',#1636,.T.);
#1183=FACE_OUTER_BOUND('',#1638,.T.);
#1184=FACE_OUTER_BOUND('',#1639,.T.);
#1185=FACE_OUTER_BOUND('',#1640,.T.);
#1186=FACE_OUTER_BOUND('',#1641,.T.);
#1187=FACE_OUTER_BOUND('',#1642,.T.);
#1188=FACE_OUTER_BOUND('',#1643,.T.);
#1189=FACE_OUTER_BOUND('',#1645,.T.);
#1190=FACE_OUTER_BOUND('',#1647,.T.);
#1191=FACE_OUTER_BOUND('',#1648,.T.);
#1192=FACE_OUTER_BOUND('',#1649,.T.);
#1193=FACE_OUTER_BOUND('',#1651,.T.);
#1194=FACE_OUTER_BOUND('',#1652,.T.);
#1195=FACE_OUTER_BOUND('',#1653,.T.);
#1196=FACE_OUTER_BOUND('',#1654,.T.);
#1197=FACE_OUTER_BOUND('',#1655,.T.);
#1198=FACE_OUTER_BOUND('',#1657,.T.);
#1199=FACE_OUTER_BOUND('',#1659,.T.);
#1200=FACE_OUTER_BOUND('',#1660,.T.);
#1201=FACE_OUTER_BOUND('',#1661,.T.);
#1202=FACE_OUTER_BOUND('',#1663,.T.);
#1203=FACE_OUTER_BOUND('',#1665,.T.);
#1204=FACE_OUTER_BOUND('',#1666,.T.);
#1205=FACE_OUTER_BOUND('',#1667,.T.);
#1206=FACE_OUTER_BOUND('',#1668,.T.);
#1207=FACE_OUTER_BOUND('',#1669,.T.);
#1208=FACE_OUTER_BOUND('',#1670,.T.);
#1209=FACE_OUTER_BOUND('',#1671,.T.);
#1210=FACE_OUTER_BOUND('',#1672,.T.);
#1211=FACE_OUTER_BOUND('',#1674,.T.);
#1212=FACE_OUTER_BOUND('',#1676,.T.);
#1213=FACE_OUTER_BOUND('',#1677,.T.);
#1214=FACE_OUTER_BOUND('',#1678,.T.);
#1215=FACE_OUTER_BOUND('',#1679,.T.);
#1216=FACE_OUTER_BOUND('',#1680,.T.);
#1217=FACE_OUTER_BOUND('',#1681,.T.);
#1218=FACE_OUTER_BOUND('',#1682,.T.);
#1219=FACE_OUTER_BOUND('',#1683,.T.);
#1220=FACE_OUTER_BOUND('',#1685,.T.);
#1221=FACE_OUTER_BOUND('',#1687,.T.);
#1222=FACE_OUTER_BOUND('',#1688,.T.);
#1223=FACE_OUTER_BOUND('',#1689,.T.);
#1224=FACE_OUTER_BOUND('',#1690,.T.);
#1225=FACE_OUTER_BOUND('',#1691,.T.);
#1226=FACE_OUTER_BOUND('',#1692,.T.);
#1227=FACE_OUTER_BOUND('',#1693,.T.);
#1228=FACE_OUTER_BOUND('',#1695,.T.);
#1229=FACE_OUTER_BOUND('',#1697,.T.);
#1230=FACE_OUTER_BOUND('',#1698,.T.);
#1231=FACE_OUTER_BOUND('',#1699,.T.);
#1232=FACE_OUTER_BOUND('',#1700,.T.);
#1233=FACE_OUTER_BOUND('',#1701,.T.);
#1234=FACE_OUTER_BOUND('',#1707,.T.);
#1235=FACE_OUTER_BOUND('',#1713,.T.);
#1236=FACE_OUTER_BOUND('',#1714,.T.);
#1237=FACE_OUTER_BOUND('',#1716,.T.);
#1238=FACE_OUTER_BOUND('',#1717,.T.);
#1239=FACE_OUTER_BOUND('',#1719,.T.);
#1240=FACE_OUTER_BOUND('',#1720,.T.);
#1241=FACE_OUTER_BOUND('',#1721,.T.);
#1242=FACE_OUTER_BOUND('',#1722,.T.);
#1243=FACE_OUTER_BOUND('',#1723,.T.);
#1244=FACE_OUTER_BOUND('',#1724,.T.);
#1245=FACE_OUTER_BOUND('',#1725,.T.);
#1246=FACE_OUTER_BOUND('',#1726,.T.);
#1247=FACE_OUTER_BOUND('',#1727,.T.);
#1248=FACE_OUTER_BOUND('',#1728,.T.);
#1249=FACE_OUTER_BOUND('',#1729,.T.);
#1250=FACE_OUTER_BOUND('',#1730,.T.);
#1251=FACE_OUTER_BOUND('',#1731,.T.);
#1252=FACE_OUTER_BOUND('',#1732,.T.);
#1253=FACE_OUTER_BOUND('',#1733,.T.);
#1254=FACE_OUTER_BOUND('',#1734,.T.);
#1255=FACE_OUTER_BOUND('',#1735,.T.);
#1256=FACE_OUTER_BOUND('',#1736,.T.);
#1257=FACE_OUTER_BOUND('',#1738,.T.);
#1258=FACE_OUTER_BOUND('',#1739,.T.);
#1259=FACE_OUTER_BOUND('',#1740,.T.);
#1260=FACE_OUTER_BOUND('',#1741,.T.);
#1261=EDGE_LOOP('',(#4330,#4331,#4332,#4333));
#1262=EDGE_LOOP('',(#4334,#4335,#4336,#4337));
#1263=EDGE_LOOP('',(#4338,#4339,#4340,#4341));
#1264=EDGE_LOOP('',(#4342,#4343,#4344,#4345));
#1265=EDGE_LOOP('',(#4346,#4347,#4348,#4349));
#1266=EDGE_LOOP('',(#4350,#4351,#4352,#4353));
#1267=EDGE_LOOP('',(#4354,#4355,#4356,#4357));
#1268=EDGE_LOOP('',(#4358,#4359,#4360,#4361));
#1269=EDGE_LOOP('',(#4362,#4363,#4364,#4365));
#1270=EDGE_LOOP('',(#4366,#4367,#4368,#4369));
#1271=EDGE_LOOP('',(#4370,#4371,#4372,#4373));
#1272=EDGE_LOOP('',(#4374,#4375,#4376,#4377));
#1273=EDGE_LOOP('',(#4378,#4379,#4380,#4381));
#1274=EDGE_LOOP('',(#4382,#4383,#4384,#4385));
#1275=EDGE_LOOP('',(#4386,#4387,#4388,#4389));
#1276=EDGE_LOOP('',(#4390,#4391,#4392,#4393));
#1277=EDGE_LOOP('',(#4394,#4395,#4396,#4397));
#1278=EDGE_LOOP('',(#4398));
#1279=EDGE_LOOP('',(#4399));
#1280=EDGE_LOOP('',(#4400));
#1281=EDGE_LOOP('',(#4401));
#1282=EDGE_LOOP('',(#4402));
#1283=EDGE_LOOP('',(#4403));
#1284=EDGE_LOOP('',(#4404));
#1285=EDGE_LOOP('',(#4405));
#1286=EDGE_LOOP('',(#4406));
#1287=EDGE_LOOP('',(#4407));
#1288=EDGE_LOOP('',(#4408));
#1289=EDGE_LOOP('',(#4409));
#1290=EDGE_LOOP('',(#4410,#4411,#4412,#4413));
#1291=EDGE_LOOP('',(#4414));
#1292=EDGE_LOOP('',(#4415));
#1293=EDGE_LOOP('',(#4416));
#1294=EDGE_LOOP('',(#4417));
#1295=EDGE_LOOP('',(#4418));
#1296=EDGE_LOOP('',(#4419));
#1297=EDGE_LOOP('',(#4420));
#1298=EDGE_LOOP('',(#4421));
#1299=EDGE_LOOP('',(#4422));
#1300=EDGE_LOOP('',(#4423));
#1301=EDGE_LOOP('',(#4424));
#1302=EDGE_LOOP('',(#4425));
#1303=EDGE_LOOP('',(#4426,#4427,#4428,#4429));
#1304=EDGE_LOOP('',(#4430,#4431,#4432,#4433));
#1305=EDGE_LOOP('',(#4434,#4435,#4436,#4437));
#1306=EDGE_LOOP('',(#4438,#4439,#4440,#4441));
#1307=EDGE_LOOP('',(#4442,#4443,#4444,#4445));
#1308=EDGE_LOOP('',(#4446,#4447,#4448,#4449));
#1309=EDGE_LOOP('',(#4450,#4451,#4452,#4453));
#1310=EDGE_LOOP('',(#4454,#4455,#4456,#4457));
#1311=EDGE_LOOP('',(#4458,#4459,#4460,#4461));
#1312=EDGE_LOOP('',(#4462,#4463,#4464,#4465));
#1313=EDGE_LOOP('',(#4466,#4467,#4468,#4469));
#1314=EDGE_LOOP('',(#4470,#4471,#4472,#4473));
#1315=EDGE_LOOP('',(#4474,#4475,#4476,#4477));
#1316=EDGE_LOOP('',(#4478,#4479,#4480,#4481));
#1317=EDGE_LOOP('',(#4482,#4483,#4484,#4485));
#1318=EDGE_LOOP('',(#4486,#4487,#4488,#4489));
#1319=EDGE_LOOP('',(#4490,#4491,#4492,#4493));
#1320=EDGE_LOOP('',(#4494,#4495,#4496,#4497));
#1321=EDGE_LOOP('',(#4498,#4499,#4500,#4501));
#1322=EDGE_LOOP('',(#4502,#4503,#4504,#4505));
#1323=EDGE_LOOP('',(#4506,#4507,#4508,#4509));
#1324=EDGE_LOOP('',(#4510,#4511,#4512,#4513));
#1325=EDGE_LOOP('',(#4514,#4515,#4516,#4517));
#1326=EDGE_LOOP('',(#4518,#4519,#4520,#4521));
#1327=EDGE_LOOP('',(#4522,#4523,#4524,#4525));
#1328=EDGE_LOOP('',(#4526,#4527,#4528,#4529));
#1329=EDGE_LOOP('',(#4530,#4531,#4532,#4533));
#1330=EDGE_LOOP('',(#4534,#4535,#4536,#4537));
#1331=EDGE_LOOP('',(#4538,#4539,#4540,#4541));
#1332=EDGE_LOOP('',(#4542,#4543,#4544,#4545));
#1333=EDGE_LOOP('',(#4546,#4547,#4548,#4549));
#1334=EDGE_LOOP('',(#4550,#4551,#4552,#4553));
#1335=EDGE_LOOP('',(#4554));
#1336=EDGE_LOOP('',(#4555));
#1337=EDGE_LOOP('',(#4556,#4557,#4558,#4559));
#1338=EDGE_LOOP('',(#4560,#4561,#4562,#4563));
#1339=EDGE_LOOP('',(#4564));
#1340=EDGE_LOOP('',(#4565));
#1341=EDGE_LOOP('',(#4566));
#1342=EDGE_LOOP('',(#4567));
#1343=EDGE_LOOP('',(#4568));
#1344=EDGE_LOOP('',(#4569,#4570,#4571,#4572,#4573,#4574));
#1345=EDGE_LOOP('',(#4575,#4576,#4577,#4578,#4579,#4580));
#1346=EDGE_LOOP('',(#4581,#4582,#4583,#4584));
#1347=EDGE_LOOP('',(#4585));
#1348=EDGE_LOOP('',(#4586));
#1349=EDGE_LOOP('',(#4587));
#1350=EDGE_LOOP('',(#4588));
#1351=EDGE_LOOP('',(#4589));
#1352=EDGE_LOOP('',(#4590,#4591,#4592,#4593));
#1353=EDGE_LOOP('',(#4594,#4595,#4596,#4597));
#1354=EDGE_LOOP('',(#4598));
#1355=EDGE_LOOP('',(#4599));
#1356=EDGE_LOOP('',(#4600,#4601,#4602,#4603));
#1357=EDGE_LOOP('',(#4604,#4605,#4606,#4607));
#1358=EDGE_LOOP('',(#4608));
#1359=EDGE_LOOP('',(#4609));
#1360=EDGE_LOOP('',(#4610));
#1361=EDGE_LOOP('',(#4611));
#1362=EDGE_LOOP('',(#4612,#4613,#4614,#4615));
#1363=EDGE_LOOP('',(#4616,#4617,#4618,#4619));
#1364=EDGE_LOOP('',(#4620));
#1365=EDGE_LOOP('',(#4621));
#1366=EDGE_LOOP('',(#4622));
#1367=EDGE_LOOP('',(#4623));
#1368=EDGE_LOOP('',(#4624,#4625,#4626,#4627));
#1369=EDGE_LOOP('',(#4628,#4629,#4630,#4631));
#1370=EDGE_LOOP('',(#4632));
#1371=EDGE_LOOP('',(#4633));
#1372=EDGE_LOOP('',(#4634));
#1373=EDGE_LOOP('',(#4635));
#1374=EDGE_LOOP('',(#4636,#4637,#4638,#4639));
#1375=EDGE_LOOP('',(#4640,#4641,#4642,#4643));
#1376=EDGE_LOOP('',(#4644));
#1377=EDGE_LOOP('',(#4645));
#1378=EDGE_LOOP('',(#4646));
#1379=EDGE_LOOP('',(#4647));
#1380=EDGE_LOOP('',(#4648,#4649,#4650,#4651));
#1381=EDGE_LOOP('',(#4652,#4653,#4654,#4655));
#1382=EDGE_LOOP('',(#4656,#4657,#4658,#4659));
#1383=EDGE_LOOP('',(#4660,#4661,#4662,#4663));
#1384=EDGE_LOOP('',(#4664,#4665,#4666,#4667));
#1385=EDGE_LOOP('',(#4668,#4669,#4670,#4671));
#1386=EDGE_LOOP('',(#4672,#4673,#4674,#4675));
#1387=EDGE_LOOP('',(#4676,#4677,#4678,#4679));
#1388=EDGE_LOOP('',(#4680));
#1389=EDGE_LOOP('',(#4681));
#1390=EDGE_LOOP('',(#4682,#4683,#4684,#4685));
#1391=EDGE_LOOP('',(#4686,#4687,#4688,#4689));
#1392=EDGE_LOOP('',(#4690));
#1393=EDGE_LOOP('',(#4691));
#1394=EDGE_LOOP('',(#4692));
#1395=EDGE_LOOP('',(#4693));
#1396=EDGE_LOOP('',(#4694));
#1397=EDGE_LOOP('',(#4695,#4696,#4697,#4698,#4699,#4700));
#1398=EDGE_LOOP('',(#4701,#4702,#4703,#4704,#4705,#4706));
#1399=EDGE_LOOP('',(#4707,#4708,#4709,#4710));
#1400=EDGE_LOOP('',(#4711));
#1401=EDGE_LOOP('',(#4712));
#1402=EDGE_LOOP('',(#4713));
#1403=EDGE_LOOP('',(#4714));
#1404=EDGE_LOOP('',(#4715));
#1405=EDGE_LOOP('',(#4716,#4717,#4718,#4719));
#1406=EDGE_LOOP('',(#4720,#4721,#4722,#4723));
#1407=EDGE_LOOP('',(#4724));
#1408=EDGE_LOOP('',(#4725));
#1409=EDGE_LOOP('',(#4726,#4727,#4728,#4729));
#1410=EDGE_LOOP('',(#4730,#4731,#4732,#4733));
#1411=EDGE_LOOP('',(#4734));
#1412=EDGE_LOOP('',(#4735));
#1413=EDGE_LOOP('',(#4736));
#1414=EDGE_LOOP('',(#4737));
#1415=EDGE_LOOP('',(#4738,#4739,#4740,#4741));
#1416=EDGE_LOOP('',(#4742,#4743,#4744,#4745));
#1417=EDGE_LOOP('',(#4746));
#1418=EDGE_LOOP('',(#4747));
#1419=EDGE_LOOP('',(#4748));
#1420=EDGE_LOOP('',(#4749));
#1421=EDGE_LOOP('',(#4750,#4751,#4752,#4753));
#1422=EDGE_LOOP('',(#4754,#4755,#4756,#4757));
#1423=EDGE_LOOP('',(#4758));
#1424=EDGE_LOOP('',(#4759));
#1425=EDGE_LOOP('',(#4760));
#1426=EDGE_LOOP('',(#4761));
#1427=EDGE_LOOP('',(#4762,#4763,#4764,#4765));
#1428=EDGE_LOOP('',(#4766,#4767,#4768,#4769));
#1429=EDGE_LOOP('',(#4770));
#1430=EDGE_LOOP('',(#4771));
#1431=EDGE_LOOP('',(#4772));
#1432=EDGE_LOOP('',(#4773));
#1433=EDGE_LOOP('',(#4774,#4775,#4776,#4777));
#1434=EDGE_LOOP('',(#4778,#4779,#4780,#4781));
#1435=EDGE_LOOP('',(#4782,#4783,#4784,#4785));
#1436=EDGE_LOOP('',(#4786,#4787,#4788,#4789));
#1437=EDGE_LOOP('',(#4790,#4791,#4792,#4793));
#1438=EDGE_LOOP('',(#4794,#4795,#4796,#4797));
#1439=EDGE_LOOP('',(#4798,#4799,#4800,#4801));
#1440=EDGE_LOOP('',(#4802,#4803,#4804,#4805));
#1441=EDGE_LOOP('',(#4806,#4807,#4808,#4809));
#1442=EDGE_LOOP('',(#4810,#4811,#4812,#4813));
#1443=EDGE_LOOP('',(#4814,#4815,#4816,#4817));
#1444=EDGE_LOOP('',(#4818,#4819,#4820,#4821));
#1445=EDGE_LOOP('',(#4822,#4823,#4824,#4825));
#1446=EDGE_LOOP('',(#4826,#4827,#4828,#4829));
#1447=EDGE_LOOP('',(#4830,#4831,#4832,#4833));
#1448=EDGE_LOOP('',(#4834,#4835,#4836,#4837));
#1449=EDGE_LOOP('',(#4838,#4839,#4840,#4841));
#1450=EDGE_LOOP('',(#4842,#4843,#4844,#4845));
#1451=EDGE_LOOP('',(#4846,#4847,#4848,#4849));
#1452=EDGE_LOOP('',(#4850,#4851,#4852,#4853));
#1453=EDGE_LOOP('',(#4854,#4855,#4856,#4857));
#1454=EDGE_LOOP('',(#4858,#4859,#4860,#4861));
#1455=EDGE_LOOP('',(#4862,#4863,#4864,#4865));
#1456=EDGE_LOOP('',(#4866,#4867,#4868,#4869));
#1457=EDGE_LOOP('',(#4870,#4871,#4872,#4873));
#1458=EDGE_LOOP('',(#4874,#4875,#4876,#4877));
#1459=EDGE_LOOP('',(#4878,#4879,#4880,#4881));
#1460=EDGE_LOOP('',(#4882,#4883,#4884,#4885));
#1461=EDGE_LOOP('',(#4886,#4887,#4888,#4889));
#1462=EDGE_LOOP('',(#4890,#4891,#4892,#4893));
#1463=EDGE_LOOP('',(#4894,#4895,#4896,#4897));
#1464=EDGE_LOOP('',(#4898,#4899,#4900,#4901));
#1465=EDGE_LOOP('',(#4902,#4903,#4904,#4905));
#1466=EDGE_LOOP('',(#4906,#4907,#4908,#4909));
#1467=EDGE_LOOP('',(#4910,#4911,#4912,#4913));
#1468=EDGE_LOOP('',(#4914,#4915,#4916,#4917));
#1469=EDGE_LOOP('',(#4918,#4919,#4920,#4921));
#1470=EDGE_LOOP('',(#4922,#4923,#4924,#4925));
#1471=EDGE_LOOP('',(#4926,#4927,#4928,#4929));
#1472=EDGE_LOOP('',(#4930,#4931,#4932,#4933));
#1473=EDGE_LOOP('',(#4934,#4935,#4936,#4937));
#1474=EDGE_LOOP('',(#4938,#4939,#4940,#4941));
#1475=EDGE_LOOP('',(#4942,#4943,#4944,#4945));
#1476=EDGE_LOOP('',(#4946,#4947,#4948,#4949));
#1477=EDGE_LOOP('',(#4950,#4951,#4952,#4953));
#1478=EDGE_LOOP('',(#4954,#4955,#4956,#4957,#4958,#4959,#4960,#4961,#4962,
#4963,#4964,#4965,#4966,#4967,#4968,#4969,#4970,#4971,#4972,#4973,#4974,
#4975,#4976,#4977,#4978,#4979,#4980,#4981,#4982,#4983,#4984,#4985,#4986,
#4987,#4988,#4989,#4990,#4991,#4992,#4993,#4994,#4995,#4996,#4997));
#1479=EDGE_LOOP('',(#4998));
#1480=EDGE_LOOP('',(#4999,#5000,#5001,#5002,#5003,#5004,#5005,#5006,#5007,
#5008,#5009,#5010,#5011,#5012,#5013,#5014,#5015,#5016,#5017,#5018,#5019,
#5020,#5021,#5022,#5023,#5024,#5025,#5026,#5027,#5028,#5029,#5030,#5031,
#5032,#5033,#5034,#5035,#5036,#5037,#5038,#5039,#5040,#5041,#5042));
#1481=EDGE_LOOP('',(#5043));
#1482=EDGE_LOOP('',(#5044,#5045,#5046,#5047));
#1483=EDGE_LOOP('',(#5048,#5049,#5050,#5051));
#1484=EDGE_LOOP('',(#5052,#5053,#5054,#5055));
#1485=EDGE_LOOP('',(#5056));
#1486=EDGE_LOOP('',(#5057,#5058,#5059,#5060,#5061,#5062,#5063,#5064,#5065,
#5066));
#1487=EDGE_LOOP('',(#5067,#5068,#5069,#5070));
#1488=EDGE_LOOP('',(#5071,#5072,#5073,#5074));
#1489=EDGE_LOOP('',(#5075,#5076,#5077,#5078,#5079,#5080,#5081,#5082,#5083,
#5084));
#1490=EDGE_LOOP('',(#5085,#5086,#5087,#5088));
#1491=EDGE_LOOP('',(#5089,#5090,#5091,#5092,#5093,#5094));
#1492=EDGE_LOOP('',(#5095,#5096,#5097,#5098,#5099,#5100,#5101,#5102));
#1493=EDGE_LOOP('',(#5103,#5104,#5105,#5106,#5107));
#1494=EDGE_LOOP('',(#5108,#5109,#5110,#5111));
#1495=EDGE_LOOP('',(#5112,#5113,#5114,#5115,#5116,#5117));
#1496=EDGE_LOOP('',(#5118,#5119,#5120,#5121));
#1497=EDGE_LOOP('',(#5122,#5123,#5124,#5125));
#1498=EDGE_LOOP('',(#5126,#5127,#5128,#5129));
#1499=EDGE_LOOP('',(#5130,#5131,#5132,#5133));
#1500=EDGE_LOOP('',(#5134,#5135,#5136,#5137));
#1501=EDGE_LOOP('',(#5138,#5139,#5140,#5141));
#1502=EDGE_LOOP('',(#5142,#5143,#5144,#5145));
#1503=EDGE_LOOP('',(#5146,#5147,#5148,#5149,#5150,#5151));
#1504=EDGE_LOOP('',(#5152,#5153,#5154,#5155,#5156,#5157));
#1505=EDGE_LOOP('',(#5158));
#1506=EDGE_LOOP('',(#5159));
#1507=EDGE_LOOP('',(#5160,#5161,#5162,#5163));
#1508=EDGE_LOOP('',(#5164,#5165,#5166,#5167));
#1509=EDGE_LOOP('',(#5168,#5169,#5170,#5171));
#1510=EDGE_LOOP('',(#5172));
#1511=EDGE_LOOP('',(#5173));
#1512=EDGE_LOOP('',(#5174,#5175,#5176,#5177));
#1513=EDGE_LOOP('',(#5178,#5179,#5180,#5181));
#1514=EDGE_LOOP('',(#5182,#5183,#5184,#5185));
#1515=EDGE_LOOP('',(#5186,#5187,#5188,#5189));
#1516=EDGE_LOOP('',(#5190,#5191,#5192,#5193));
#1517=EDGE_LOOP('',(#5194,#5195,#5196,#5197));
#1518=EDGE_LOOP('',(#5198,#5199,#5200,#5201));
#1519=EDGE_LOOP('',(#5202,#5203,#5204,#5205));
#1520=EDGE_LOOP('',(#5206,#5207,#5208,#5209,#5210,#5211));
#1521=EDGE_LOOP('',(#5212,#5213,#5214,#5215,#5216,#5217));
#1522=EDGE_LOOP('',(#5218));
#1523=EDGE_LOOP('',(#5219));
#1524=EDGE_LOOP('',(#5220,#5221,#5222,#5223));
#1525=EDGE_LOOP('',(#5224,#5225,#5226,#5227));
#1526=EDGE_LOOP('',(#5228,#5229,#5230,#5231));
#1527=EDGE_LOOP('',(#5232));
#1528=EDGE_LOOP('',(#5233));
#1529=EDGE_LOOP('',(#5234,#5235,#5236,#5237));
#1530=EDGE_LOOP('',(#5238,#5239,#5240,#5241));
#1531=EDGE_LOOP('',(#5242,#5243,#5244,#5245));
#1532=EDGE_LOOP('',(#5246,#5247,#5248,#5249));
#1533=EDGE_LOOP('',(#5250,#5251));
#1534=EDGE_LOOP('',(#5252));
#1535=EDGE_LOOP('',(#5253));
#1536=EDGE_LOOP('',(#5254,#5255,#5256,#5257));
#1537=EDGE_LOOP('',(#5258,#5259,#5260,#5261));
#1538=EDGE_LOOP('',(#5262));
#1539=EDGE_LOOP('',(#5263));
#1540=EDGE_LOOP('',(#5264));
#1541=EDGE_LOOP('',(#5265));
#1542=EDGE_LOOP('',(#5266,#5267,#5268,#5269));
#1543=EDGE_LOOP('',(#5270,#5271,#5272,#5273));
#1544=EDGE_LOOP('',(#5274,#5275,#5276,#5277));
#1545=EDGE_LOOP('',(#5278,#5279,#5280,#5281));
#1546=EDGE_LOOP('',(#5282,#5283,#5284,#5285));
#1547=EDGE_LOOP('',(#5286,#5287,#5288,#5289));
#1548=EDGE_LOOP('',(#5290,#5291,#5292,#5293));
#1549=EDGE_LOOP('',(#5294,#5295,#5296,#5297));
#1550=EDGE_LOOP('',(#5298,#5299,#5300,#5301));
#1551=EDGE_LOOP('',(#5302,#5303,#5304,#5305));
#1552=EDGE_LOOP('',(#5306,#5307,#5308,#5309));
#1553=EDGE_LOOP('',(#5310,#5311,#5312,#5313));
#1554=EDGE_LOOP('',(#5314,#5315,#5316,#5317,#5318,#5319,#5320,#5321));
#1555=EDGE_LOOP('',(#5322));
#1556=EDGE_LOOP('',(#5323));
#1557=EDGE_LOOP('',(#5324));
#1558=EDGE_LOOP('',(#5325));
#1559=EDGE_LOOP('',(#5326));
#1560=EDGE_LOOP('',(#5327,#5328,#5329,#5330,#5331,#5332,#5333,#5334));
#1561=EDGE_LOOP('',(#5335));
#1562=EDGE_LOOP('',(#5336));
#1563=EDGE_LOOP('',(#5337));
#1564=EDGE_LOOP('',(#5338));
#1565=EDGE_LOOP('',(#5339));
#1566=EDGE_LOOP('',(#5340,#5341,#5342,#5343));
#1567=EDGE_LOOP('',(#5344));
#1568=EDGE_LOOP('',(#5345));
#1569=EDGE_LOOP('',(#5346,#5347));
#1570=EDGE_LOOP('',(#5348));
#1571=EDGE_LOOP('',(#5349));
#1572=EDGE_LOOP('',(#5350));
#1573=EDGE_LOOP('',(#5351));
#1574=EDGE_LOOP('',(#5352,#5353,#5354,#5355,#5356,#5357));
#1575=EDGE_LOOP('',(#5358,#5359,#5360,#5361,#5362,#5363));
#1576=EDGE_LOOP('',(#5364,#5365,#5366,#5367));
#1577=EDGE_LOOP('',(#5368,#5369,#5370));
#1578=EDGE_LOOP('',(#5371,#5372,#5373));
#1579=EDGE_LOOP('',(#5374,#5375,#5376));
#1580=EDGE_LOOP('',(#5377,#5378,#5379));
#1581=EDGE_LOOP('',(#5380,#5381,#5382));
#1582=EDGE_LOOP('',(#5383,#5384,#5385));
#1583=EDGE_LOOP('',(#5386,#5387,#5388,#5389,#5390,#5391));
#1584=EDGE_LOOP('',(#5392,#5393,#5394,#5395,#5396,#5397));
#1585=EDGE_LOOP('',(#5398,#5399,#5400,#5401,#5402,#5403));
#1586=EDGE_LOOP('',(#5404,#5405,#5406,#5407,#5408,#5409));
#1587=EDGE_LOOP('',(#5410));
#1588=EDGE_LOOP('',(#5411));
#1589=EDGE_LOOP('',(#5412));
#1590=EDGE_LOOP('',(#5413));
#1591=EDGE_LOOP('',(#5414,#5415,#5416,#5417));
#1592=EDGE_LOOP('',(#5418));
#1593=EDGE_LOOP('',(#5419));
#1594=EDGE_LOOP('',(#5420,#5421,#5422,#5423));
#1595=EDGE_LOOP('',(#5424));
#1596=EDGE_LOOP('',(#5425));
#1597=EDGE_LOOP('',(#5426));
#1598=EDGE_LOOP('',(#5427));
#1599=EDGE_LOOP('',(#5428));
#1600=EDGE_LOOP('',(#5429));
#1601=EDGE_LOOP('',(#5430));
#1602=EDGE_LOOP('',(#5431,#5432,#5433,#5434));
#1603=EDGE_LOOP('',(#5435,#5436,#5437,#5438));
#1604=EDGE_LOOP('',(#5439,#5440,#5441,#5442));
#1605=EDGE_LOOP('',(#5443));
#1606=EDGE_LOOP('',(#5444));
#1607=EDGE_LOOP('',(#5445,#5446,#5447,#5448));
#1608=EDGE_LOOP('',(#5449,#5450,#5451,#5452));
#1609=EDGE_LOOP('',(#5453,#5454,#5455,#5456));
#1610=EDGE_LOOP('',(#5457));
#1611=EDGE_LOOP('',(#5458,#5459,#5460,#5461));
#1612=EDGE_LOOP('',(#5462,#5463,#5464,#5465));
#1613=EDGE_LOOP('',(#5466,#5467,#5468,#5469));
#1614=EDGE_LOOP('',(#5470,#5471,#5472,#5473));
#1615=EDGE_LOOP('',(#5474,#5475,#5476,#5477));
#1616=EDGE_LOOP('',(#5478,#5479,#5480,#5481));
#1617=EDGE_LOOP('',(#5482,#5483,#5484,#5485,#5486,#5487));
#1618=EDGE_LOOP('',(#5488,#5489,#5490,#5491,#5492,#5493));
#1619=EDGE_LOOP('',(#5494,#5495,#5496,#5497));
#1620=EDGE_LOOP('',(#5498,#5499,#5500,#5501));
#1621=EDGE_LOOP('',(#5502));
#1622=EDGE_LOOP('',(#5503));
#1623=EDGE_LOOP('',(#5504));
#1624=EDGE_LOOP('',(#5505));
#1625=EDGE_LOOP('',(#5506,#5507,#5508,#5509,#5510,#5511,#5512,#5513,#5514));
#1626=EDGE_LOOP('',(#5515,#5516,#5517,#5518,#5519,#5520,#5521,#5522,#5523));
#1627=EDGE_LOOP('',(#5524,#5525,#5526,#5527));
#1628=EDGE_LOOP('',(#5528,#5529,#5530,#5531));
#1629=EDGE_LOOP('',(#5532,#5533,#5534,#5535));
#1630=EDGE_LOOP('',(#5536,#5537,#5538,#5539));
#1631=EDGE_LOOP('',(#5540,#5541,#5542,#5543));
#1632=EDGE_LOOP('',(#5544,#5545,#5546,#5547));
#1633=EDGE_LOOP('',(#5548,#5549,#5550,#5551));
#1634=EDGE_LOOP('',(#5552));
#1635=EDGE_LOOP('',(#5553));
#1636=EDGE_LOOP('',(#5554));
#1637=EDGE_LOOP('',(#5555));
#1638=EDGE_LOOP('',(#5556,#5557,#5558,#5559));
#1639=EDGE_LOOP('',(#5560,#5561,#5562,#5563));
#1640=EDGE_LOOP('',(#5564,#5565,#5566,#5567));
#1641=EDGE_LOOP('',(#5568,#5569,#5570,#5571));
#1642=EDGE_LOOP('',(#5572,#5573,#5574,#5575));
#1643=EDGE_LOOP('',(#5576));
#1644=EDGE_LOOP('',(#5577));
#1645=EDGE_LOOP('',(#5578));
#1646=EDGE_LOOP('',(#5579));
#1647=EDGE_LOOP('',(#5580,#5581,#5582,#5583));
#1648=EDGE_LOOP('',(#5584,#5585,#5586,#5587));
#1649=EDGE_LOOP('',(#5588,#5589,#5590,#5591));
#1650=EDGE_LOOP('',(#5592,#5593,#5594,#5595));
#1651=EDGE_LOOP('',(#5596));
#1652=EDGE_LOOP('',(#5597));
#1653=EDGE_LOOP('',(#5598,#5599,#5600,#5601));
#1654=EDGE_LOOP('',(#5602,#5603,#5604,#5605));
#1655=EDGE_LOOP('',(#5606));
#1656=EDGE_LOOP('',(#5607));
#1657=EDGE_LOOP('',(#5608));
#1658=EDGE_LOOP('',(#5609));
#1659=EDGE_LOOP('',(#5610,#5611,#5612,#5613));
#1660=EDGE_LOOP('',(#5614,#5615,#5616,#5617));
#1661=EDGE_LOOP('',(#5618));
#1662=EDGE_LOOP('',(#5619));
#1663=EDGE_LOOP('',(#5620));
#1664=EDGE_LOOP('',(#5621));
#1665=EDGE_LOOP('',(#5622,#5623,#5624,#5625));
#1666=EDGE_LOOP('',(#5626,#5627,#5628,#5629));
#1667=EDGE_LOOP('',(#5630,#5631,#5632,#5633));
#1668=EDGE_LOOP('',(#5634,#5635,#5636,#5637));
#1669=EDGE_LOOP('',(#5638,#5639,#5640,#5641));
#1670=EDGE_LOOP('',(#5642,#5643,#5644,#5645));
#1671=EDGE_LOOP('',(#5646,#5647,#5648,#5649));
#1672=EDGE_LOOP('',(#5650,#5651,#5652,#5653,#5654,#5655));
#1673=EDGE_LOOP('',(#5656));
#1674=EDGE_LOOP('',(#5657,#5658,#5659,#5660,#5661,#5662));
#1675=EDGE_LOOP('',(#5663));
#1676=EDGE_LOOP('',(#5664,#5665,#5666,#5667));
#1677=EDGE_LOOP('',(#5668,#5669,#5670,#5671));
#1678=EDGE_LOOP('',(#5672,#5673,#5674,#5675));
#1679=EDGE_LOOP('',(#5676,#5677,#5678,#5679));
#1680=EDGE_LOOP('',(#5680,#5681,#5682,#5683));
#1681=EDGE_LOOP('',(#5684,#5685,#5686,#5687));
#1682=EDGE_LOOP('',(#5688,#5689,#5690,#5691));
#1683=EDGE_LOOP('',(#5692,#5693,#5694,#5695,#5696,#5697));
#1684=EDGE_LOOP('',(#5698));
#1685=EDGE_LOOP('',(#5699,#5700,#5701,#5702,#5703,#5704));
#1686=EDGE_LOOP('',(#5705));
#1687=EDGE_LOOP('',(#5706,#5707));
#1688=EDGE_LOOP('',(#5708,#5709,#5710,#5711,#5712,#5713,#5714,#5715,#5716));
#1689=EDGE_LOOP('',(#5717,#5718,#5719));
#1690=EDGE_LOOP('',(#5720,#5721,#5722,#5723));
#1691=EDGE_LOOP('',(#5724,#5725,#5726,#5727));
#1692=EDGE_LOOP('',(#5728,#5729,#5730,#5731));
#1693=EDGE_LOOP('',(#5732));
#1694=EDGE_LOOP('',(#5733,#5734,#5735,#5736));
#1695=EDGE_LOOP('',(#5737,#5738,#5739,#5740));
#1696=EDGE_LOOP('',(#5741,#5742,#5743,#5744));
#1697=EDGE_LOOP('',(#5745,#5746,#5747,#5748));
#1698=EDGE_LOOP('',(#5749,#5750,#5751,#5752));
#1699=EDGE_LOOP('',(#5753,#5754,#5755,#5756));
#1700=EDGE_LOOP('',(#5757,#5758,#5759,#5760));
#1701=EDGE_LOOP('',(#5761));
#1702=EDGE_LOOP('',(#5762));
#1703=EDGE_LOOP('',(#5763));
#1704=EDGE_LOOP('',(#5764));
#1705=EDGE_LOOP('',(#5765));
#1706=EDGE_LOOP('',(#5766));
#1707=EDGE_LOOP('',(#5767));
#1708=EDGE_LOOP('',(#5768));
#1709=EDGE_LOOP('',(#5769));
#1710=EDGE_LOOP('',(#5770));
#1711=EDGE_LOOP('',(#5771));
#1712=EDGE_LOOP('',(#5772));
#1713=EDGE_LOOP('',(#5773,#5774,#5775,#5776));
#1714=EDGE_LOOP('',(#5777,#5778,#5779,#5780));
#1715=EDGE_LOOP('',(#5781,#5782));
#1716=EDGE_LOOP('',(#5783,#5784,#5785,#5786));
#1717=EDGE_LOOP('',(#5787));
#1718=EDGE_LOOP('',(#5788,#5789,#5790,#5791));
#1719=EDGE_LOOP('',(#5792,#5793,#5794,#5795,#5796,#5797,#5798,#5799));
#1720=EDGE_LOOP('',(#5800,#5801,#5802,#5803));
#1721=EDGE_LOOP('',(#5804,#5805,#5806,#5807));
#1722=EDGE_LOOP('',(#5808,#5809,#5810,#5811));
#1723=EDGE_LOOP('',(#5812,#5813,#5814,#5815));
#1724=EDGE_LOOP('',(#5816,#5817,#5818,#5819,#5820,#5821,#5822,#5823));
#1725=EDGE_LOOP('',(#5824,#5825,#5826,#5827));
#1726=EDGE_LOOP('',(#5828,#5829,#5830,#5831));
#1727=EDGE_LOOP('',(#5832,#5833,#5834,#5835));
#1728=EDGE_LOOP('',(#5836,#5837,#5838,#5839));
#1729=EDGE_LOOP('',(#5840,#5841,#5842,#5843));
#1730=EDGE_LOOP('',(#5844,#5845,#5846,#5847));
#1731=EDGE_LOOP('',(#5848,#5849,#5850,#5851));
#1732=EDGE_LOOP('',(#5852,#5853,#5854,#5855));
#1733=EDGE_LOOP('',(#5856,#5857,#5858,#5859));
#1734=EDGE_LOOP('',(#5860,#5861,#5862,#5863));
#1735=EDGE_LOOP('',(#5864,#5865,#5866,#5867,#5868,#5869));
#1736=EDGE_LOOP('',(#5870));
#1737=EDGE_LOOP('',(#5871,#5872,#5873,#5874,#5875,#5876));
#1738=EDGE_LOOP('',(#5877,#5878,#5879,#5880));
#1739=EDGE_LOOP('',(#5881,#5882,#5883,#5884));
#1740=EDGE_LOOP('',(#5885,#5886,#5887,#5888));
#1741=EDGE_LOOP('',(#5889));
#1742=LINE('',#9241,#2289);
#1743=LINE('',#9247,#2290);
#1744=LINE('',#9253,#2291);
#1745=LINE('',#9259,#2292);
#1746=LINE('',#9265,#2293);
#1747=LINE('',#9271,#2294);
#1748=LINE('',#9277,#2295);
#1749=LINE('',#9283,#2296);
#1750=LINE('',#9289,#2297);
#1751=LINE('',#9295,#2298);
#1752=LINE('',#9301,#2299);
#1753=LINE('',#9307,#2300);
#1754=LINE('',#9312,#2301);
#1755=LINE('',#9314,#2302);
#1756=LINE('',#9316,#2303);
#1757=LINE('',#9317,#2304);
#1758=LINE('',#9320,#2305);
#1759=LINE('',#9322,#2306);
#1760=LINE('',#9323,#2307);
#1761=LINE('',#9326,#2308);
#1762=LINE('',#9328,#2309);
#1763=LINE('',#9329,#2310);
#1764=LINE('',#9331,#2311);
#1765=LINE('',#9332,#2312);
#1766=LINE('',#9339,#2313);
#1767=LINE('',#9341,#2314);
#1768=LINE('',#9343,#2315);
#1769=LINE('',#9344,#2316);
#1770=LINE('',#9347,#2317);
#1771=LINE('',#9349,#2318);
#1772=LINE('',#9350,#2319);
#1773=LINE('',#9353,#2320);
#1774=LINE('',#9355,#2321);
#1775=LINE('',#9356,#2322);
#1776=LINE('',#9358,#2323);
#1777=LINE('',#9359,#2324);
#1778=LINE('',#9366,#2325);
#1779=LINE('',#9368,#2326);
#1780=LINE('',#9370,#2327);
#1781=LINE('',#9371,#2328);
#1782=LINE('',#9374,#2329);
#1783=LINE('',#9376,#2330);
#1784=LINE('',#9377,#2331);
#1785=LINE('',#9380,#2332);
#1786=LINE('',#9382,#2333);
#1787=LINE('',#9383,#2334);
#1788=LINE('',#9385,#2335);
#1789=LINE('',#9386,#2336);
#1790=LINE('',#9393,#2337);
#1791=LINE('',#9395,#2338);
#1792=LINE('',#9397,#2339);
#1793=LINE('',#9398,#2340);
#1794=LINE('',#9401,#2341);
#1795=LINE('',#9403,#2342);
#1796=LINE('',#9404,#2343);
#1797=LINE('',#9407,#2344);
#1798=LINE('',#9409,#2345);
#1799=LINE('',#9410,#2346);
#1800=LINE('',#9412,#2347);
#1801=LINE('',#9413,#2348);
#1802=LINE('',#9420,#2349);
#1803=LINE('',#9422,#2350);
#1804=LINE('',#9424,#2351);
#1805=LINE('',#9425,#2352);
#1806=LINE('',#9428,#2353);
#1807=LINE('',#9430,#2354);
#1808=LINE('',#9431,#2355);
#1809=LINE('',#9434,#2356);
#1810=LINE('',#9436,#2357);
#1811=LINE('',#9437,#2358);
#1812=LINE('',#9439,#2359);
#1813=LINE('',#9440,#2360);
#1814=LINE('',#9448,#2361);
#1815=LINE('',#9454,#2362);
#1816=LINE('',#9460,#2363);
#1817=LINE('',#9466,#2364);
#1818=LINE('',#9472,#2365);
#1819=LINE('',#9478,#2366);
#1820=LINE('',#9484,#2367);
#1821=LINE('',#9489,#2368);
#1822=LINE('',#9491,#2369);
#1823=LINE('',#9493,#2370);
#1824=LINE('',#9494,#2371);
#1825=LINE('',#9497,#2372);
#1826=LINE('',#9499,#2373);
#1827=LINE('',#9500,#2374);
#1828=LINE('',#9504,#2375);
#1829=LINE('',#9506,#2376);
#1830=LINE('',#9508,#2377);
#1831=LINE('',#9509,#2378);
#1832=LINE('',#9512,#2379);
#1833=LINE('',#9513,#2380);
#1834=LINE('',#9514,#2381);
#1835=LINE('',#9517,#2382);
#1836=LINE('',#9518,#2383);
#1837=LINE('',#9519,#2384);
#1838=LINE('',#9521,#2385);
#1839=LINE('',#9529,#2386);
#1840=LINE('',#9535,#2387);
#1841=LINE('',#9544,#2388);
#1842=LINE('',#9550,#2389);
#1843=LINE('',#9559,#2390);
#1844=LINE('',#9565,#2391);
#1845=LINE('',#9574,#2392);
#1846=LINE('',#9580,#2393);
#1847=LINE('',#9589,#2394);
#1848=LINE('',#9595,#2395);
#1849=LINE('',#9601,#2396);
#1850=LINE('',#9607,#2397);
#1851=LINE('',#9613,#2398);
#1852=LINE('',#9619,#2399);
#1853=LINE('',#9625,#2400);
#1854=LINE('',#9630,#2401);
#1855=LINE('',#9632,#2402);
#1856=LINE('',#9634,#2403);
#1857=LINE('',#9635,#2404);
#1858=LINE('',#9638,#2405);
#1859=LINE('',#9640,#2406);
#1860=LINE('',#9641,#2407);
#1861=LINE('',#9645,#2408);
#1862=LINE('',#9647,#2409);
#1863=LINE('',#9649,#2410);
#1864=LINE('',#9650,#2411);
#1865=LINE('',#9653,#2412);
#1866=LINE('',#9654,#2413);
#1867=LINE('',#9655,#2414);
#1868=LINE('',#9658,#2415);
#1869=LINE('',#9659,#2416);
#1870=LINE('',#9660,#2417);
#1871=LINE('',#9662,#2418);
#1872=LINE('',#9670,#2419);
#1873=LINE('',#9676,#2420);
#1874=LINE('',#9685,#2421);
#1875=LINE('',#9691,#2422);
#1876=LINE('',#9700,#2423);
#1877=LINE('',#9706,#2424);
#1878=LINE('',#9715,#2425);
#1879=LINE('',#9721,#2426);
#1880=LINE('',#9729,#2427);
#1881=LINE('',#9731,#2428);
#1882=LINE('',#9733,#2429);
#1883=LINE('',#9734,#2430);
#1884=LINE('',#9737,#2431);
#1885=LINE('',#9739,#2432);
#1886=LINE('',#9740,#2433);
#1887=LINE('',#9743,#2434);
#1888=LINE('',#9745,#2435);
#1889=LINE('',#9746,#2436);
#1890=LINE('',#9749,#2437);
#1891=LINE('',#9751,#2438);
#1892=LINE('',#9752,#2439);
#1893=LINE('',#9755,#2440);
#1894=LINE('',#9757,#2441);
#1895=LINE('',#9758,#2442);
#1896=LINE('',#9761,#2443);
#1897=LINE('',#9763,#2444);
#1898=LINE('',#9764,#2445);
#1899=LINE('',#9767,#2446);
#1900=LINE('',#9769,#2447);
#1901=LINE('',#9770,#2448);
#1902=LINE('',#9773,#2449);
#1903=LINE('',#9775,#2450);
#1904=LINE('',#9776,#2451);
#1905=LINE('',#9779,#2452);
#1906=LINE('',#9781,#2453);
#1907=LINE('',#9782,#2454);
#1908=LINE('',#9786,#2455);
#1909=LINE('',#9788,#2456);
#1910=LINE('',#9790,#2457);
#1911=LINE('',#9791,#2458);
#1912=LINE('',#9794,#2459);
#1913=LINE('',#9796,#2460);
#1914=LINE('',#9797,#2461);
#1915=LINE('',#9800,#2462);
#1916=LINE('',#9802,#2463);
#1917=LINE('',#9803,#2464);
#1918=LINE('',#9806,#2465);
#1919=LINE('',#9808,#2466);
#1920=LINE('',#9809,#2467);
#1921=LINE('',#9812,#2468);
#1922=LINE('',#9814,#2469);
#1923=LINE('',#9815,#2470);
#1924=LINE('',#9818,#2471);
#1925=LINE('',#9820,#2472);
#1926=LINE('',#9821,#2473);
#1927=LINE('',#9824,#2474);
#1928=LINE('',#9826,#2475);
#1929=LINE('',#9827,#2476);
#1930=LINE('',#9830,#2477);
#1931=LINE('',#9832,#2478);
#1932=LINE('',#9833,#2479);
#1933=LINE('',#9836,#2480);
#1934=LINE('',#9838,#2481);
#1935=LINE('',#9839,#2482);
#1936=LINE('',#9843,#2483);
#1937=LINE('',#9845,#2484);
#1938=LINE('',#9847,#2485);
#1939=LINE('',#9848,#2486);
#1940=LINE('',#9851,#2487);
#1941=LINE('',#9853,#2488);
#1942=LINE('',#9854,#2489);
#1943=LINE('',#9857,#2490);
#1944=LINE('',#9859,#2491);
#1945=LINE('',#9860,#2492);
#1946=LINE('',#9863,#2493);
#1947=LINE('',#9865,#2494);
#1948=LINE('',#9866,#2495);
#1949=LINE('',#9869,#2496);
#1950=LINE('',#9871,#2497);
#1951=LINE('',#9872,#2498);
#1952=LINE('',#9875,#2499);
#1953=LINE('',#9877,#2500);
#1954=LINE('',#9878,#2501);
#1955=LINE('',#9881,#2502);
#1956=LINE('',#9883,#2503);
#1957=LINE('',#9884,#2504);
#1958=LINE('',#9887,#2505);
#1959=LINE('',#9889,#2506);
#1960=LINE('',#9890,#2507);
#1961=LINE('',#9893,#2508);
#1962=LINE('',#9895,#2509);
#1963=LINE('',#9896,#2510);
#1964=LINE('',#9900,#2511);
#1965=LINE('',#9902,#2512);
#1966=LINE('',#9904,#2513);
#1967=LINE('',#9905,#2514);
#1968=LINE('',#9908,#2515);
#1969=LINE('',#9910,#2516);
#1970=LINE('',#9911,#2517);
#1971=LINE('',#9914,#2518);
#1972=LINE('',#9916,#2519);
#1973=LINE('',#9917,#2520);
#1974=LINE('',#9920,#2521);
#1975=LINE('',#9922,#2522);
#1976=LINE('',#9923,#2523);
#1977=LINE('',#9926,#2524);
#1978=LINE('',#9928,#2525);
#1979=LINE('',#9929,#2526);
#1980=LINE('',#9932,#2527);
#1981=LINE('',#9934,#2528);
#1982=LINE('',#9935,#2529);
#1983=LINE('',#9938,#2530);
#1984=LINE('',#9940,#2531);
#1985=LINE('',#9941,#2532);
#1986=LINE('',#9944,#2533);
#1987=LINE('',#9946,#2534);
#1988=LINE('',#9947,#2535);
#1989=LINE('',#9950,#2536);
#1990=LINE('',#9952,#2537);
#1991=LINE('',#9953,#2538);
#1992=LINE('',#9958,#2539);
#1993=LINE('',#9962,#2540);
#1994=LINE('',#9964,#2541);
#1995=LINE('',#9965,#2542);
#1996=LINE('',#9968,#2543);
#1997=LINE('',#9970,#2544);
#1998=LINE('',#9971,#2545);
#1999=LINE('',#9973,#2546);
#2000=LINE('',#9974,#2547);
#2001=LINE('',#9977,#2548);
#2002=LINE('',#9979,#2549);
#2003=LINE('',#9980,#2550);
#2004=LINE('',#9982,#2551);
#2005=LINE('',#9983,#2552);
#2006=LINE('',#9986,#2553);
#2007=LINE('',#9988,#2554);
#2008=LINE('',#9989,#2555);
#2009=LINE('',#9991,#2556);
#2010=LINE('',#9992,#2557);
#2011=LINE('',#9994,#2558);
#2012=LINE('',#9995,#2559);
#2013=LINE('',#10002,#2560);
#2014=LINE('',#10004,#2561);
#2015=LINE('',#10006,#2562);
#2016=LINE('',#10007,#2563);
#2017=LINE('',#10010,#2564);
#2018=LINE('',#10012,#2565);
#2019=LINE('',#10013,#2566);
#2020=LINE('',#10016,#2567);
#2021=LINE('',#10018,#2568);
#2022=LINE('',#10019,#2569);
#2023=LINE('',#10024,#2570);
#2024=LINE('',#10026,#2571);
#2025=LINE('',#10028,#2572);
#2026=LINE('',#10030,#2573);
#2027=LINE('',#10032,#2574);
#2028=LINE('',#10034,#2575);
#2029=LINE('',#10035,#2576);
#2030=LINE('',#10038,#2577);
#2031=LINE('',#10039,#2578);
#2032=LINE('',#10042,#2579);
#2033=LINE('',#10043,#2580);
#2034=LINE('',#10046,#2581);
#2035=LINE('',#10048,#2582);
#2036=LINE('',#10050,#2583);
#2037=LINE('',#10052,#2584);
#2038=LINE('',#10053,#2585);
#2039=LINE('',#10055,#2586);
#2040=LINE('',#10058,#2587);
#2041=LINE('',#10061,#2588);
#2042=LINE('',#10065,#2589);
#2043=LINE('',#10072,#2590);
#2044=LINE('',#10074,#2591);
#2045=LINE('',#10076,#2592);
#2046=LINE('',#10082,#2593);
#2047=LINE('',#10084,#2594);
#2048=LINE('',#10086,#2595);
#2049=LINE('',#10087,#2596);
#2050=LINE('',#10090,#2597);
#2051=LINE('',#10092,#2598);
#2052=LINE('',#10093,#2599);
#2053=LINE('',#10096,#2600);
#2054=LINE('',#10098,#2601);
#2055=LINE('',#10099,#2602);
#2056=LINE('',#10102,#2603);
#2057=LINE('',#10104,#2604);
#2058=LINE('',#10105,#2605);
#2059=LINE('',#10108,#2606);
#2060=LINE('',#10110,#2607);
#2061=LINE('',#10111,#2608);
#2062=LINE('',#10113,#2609);
#2063=LINE('',#10114,#2610);
#2064=LINE('',#10126,#2611);
#2065=LINE('',#10130,#2612);
#2066=LINE('',#10134,#2613);
#2067=LINE('',#10141,#2614);
#2068=LINE('',#10143,#2615);
#2069=LINE('',#10148,#2616);
#2070=LINE('',#10150,#2617);
#2071=LINE('',#10152,#2618);
#2072=LINE('',#10153,#2619);
#2073=LINE('',#10156,#2620);
#2074=LINE('',#10158,#2621);
#2075=LINE('',#10159,#2622);
#2076=LINE('',#10162,#2623);
#2077=LINE('',#10164,#2624);
#2078=LINE('',#10165,#2625);
#2079=LINE('',#10168,#2626);
#2080=LINE('',#10170,#2627);
#2081=LINE('',#10171,#2628);
#2082=LINE('',#10174,#2629);
#2083=LINE('',#10176,#2630);
#2084=LINE('',#10177,#2631);
#2085=LINE('',#10179,#2632);
#2086=LINE('',#10180,#2633);
#2087=LINE('',#10192,#2634);
#2088=LINE('',#10196,#2635);
#2089=LINE('',#10200,#2636);
#2090=LINE('',#10207,#2637);
#2091=LINE('',#10209,#2638);
#2092=LINE('',#10216,#2639);
#2093=LINE('',#10222,#2640);
#2094=LINE('',#10232,#2641);
#2095=LINE('',#10238,#2642);
#2096=LINE('',#10246,#2643);
#2097=LINE('',#10252,#2644);
#2098=LINE('',#10258,#2645);
#2099=LINE('',#10264,#2646);
#2100=LINE('',#10269,#2647);
#2101=LINE('',#10271,#2648);
#2102=LINE('',#10273,#2649);
#2103=LINE('',#10274,#2650);
#2104=LINE('',#10277,#2651);
#2105=LINE('',#10279,#2652);
#2106=LINE('',#10280,#2653);
#2107=LINE('',#10283,#2654);
#2108=LINE('',#10285,#2655);
#2109=LINE('',#10286,#2656);
#2110=LINE('',#10289,#2657);
#2111=LINE('',#10291,#2658);
#2112=LINE('',#10292,#2659);
#2113=LINE('',#10295,#2660);
#2114=LINE('',#10297,#2661);
#2115=LINE('',#10298,#2662);
#2116=LINE('',#10301,#2663);
#2117=LINE('',#10303,#2664);
#2118=LINE('',#10304,#2665);
#2119=LINE('',#10307,#2666);
#2120=LINE('',#10309,#2667);
#2121=LINE('',#10310,#2668);
#2122=LINE('',#10312,#2669);
#2123=LINE('',#10313,#2670);
#2124=LINE('',#10321,#2671);
#2125=LINE('',#10376,#2672);
#2126=LINE('',#10448,#2673);
#2127=LINE('',#10493,#2674);
#2128=LINE('',#10661,#2675);
#2129=LINE('',#10732,#2676);
#2130=LINE('',#10735,#2677);
#2131=LINE('',#10806,#2678);
#2132=LINE('',#10816,#2679);
#2133=LINE('',#10821,#2680);
#2134=LINE('',#10831,#2681);
#2135=LINE('',#10835,#2682);
#2136=LINE('',#10839,#2683);
#2137=LINE('',#10846,#2684);
#2138=LINE('',#10850,#2685);
#2139=LINE('',#10854,#2686);
#2140=LINE('',#10859,#2687);
#2141=LINE('',#10861,#2688);
#2142=LINE('',#10863,#2689);
#2143=LINE('',#10864,#2690);
#2144=LINE('',#10867,#2691);
#2145=LINE('',#10869,#2692);
#2146=LINE('',#10870,#2693);
#2147=LINE('',#10873,#2694);
#2148=LINE('',#10875,#2695);
#2149=LINE('',#10876,#2696);
#2150=LINE('',#10879,#2697);
#2151=LINE('',#10881,#2698);
#2152=LINE('',#10882,#2699);
#2153=LINE('',#10885,#2700);
#2154=LINE('',#10887,#2701);
#2155=LINE('',#10888,#2702);
#2156=LINE('',#10890,#2703);
#2157=LINE('',#10891,#2704);
#2158=LINE('',#10899,#2705);
#2159=LINE('',#10905,#2706);
#2160=LINE('',#10921,#2707);
#2161=LINE('',#10942,#2708);
#2162=LINE('',#10967,#2709);
#2163=LINE('',#10968,#2710);
#2164=LINE('',#10970,#2711);
#2165=LINE('',#10972,#2712);
#2166=LINE('',#10977,#2713);
#2167=LINE('',#10980,#2714);
#2168=LINE('',#10982,#2715);
#2169=LINE('',#11064,#2716);
#2170=LINE('',#11066,#2717);
#2171=LINE('',#11068,#2718);
#2172=LINE('',#11069,#2719);
#2173=LINE('',#11074,#2720);
#2174=LINE('',#11075,#2721);
#2175=LINE('',#11078,#2722);
#2176=LINE('',#11080,#2723);
#2177=LINE('',#11081,#2724);
#2178=LINE('',#11083,#2725);
#2179=LINE('',#11097,#2726);
#2180=LINE('',#11100,#2727);
#2181=LINE('',#11105,#2728);
#2182=LINE('',#11113,#2729);
#2183=LINE('',#11119,#2730);
#2184=LINE('',#11128,#2731);
#2185=LINE('',#11134,#2732);
#2186=LINE('',#11143,#2733);
#2187=LINE('',#11148,#2734);
#2188=LINE('',#11150,#2735);
#2189=LINE('',#11152,#2736);
#2190=LINE('',#11153,#2737);
#2191=LINE('',#11156,#2738);
#2192=LINE('',#11158,#2739);
#2193=LINE('',#11159,#2740);
#2194=LINE('',#11162,#2741);
#2195=LINE('',#11164,#2742);
#2196=LINE('',#11165,#2743);
#2197=LINE('',#11168,#2744);
#2198=LINE('',#11170,#2745);
#2199=LINE('',#11171,#2746);
#2200=LINE('',#11174,#2747);
#2201=LINE('',#11176,#2748);
#2202=LINE('',#11177,#2749);
#2203=LINE('',#11179,#2750);
#2204=LINE('',#11180,#2751);
#2205=LINE('',#11188,#2752);
#2206=LINE('',#11193,#2753);
#2207=LINE('',#11195,#2754);
#2208=LINE('',#11197,#2755);
#2209=LINE('',#11198,#2756);
#2210=LINE('',#11201,#2757);
#2211=LINE('',#11203,#2758);
#2212=LINE('',#11204,#2759);
#2213=LINE('',#11207,#2760);
#2214=LINE('',#11209,#2761);
#2215=LINE('',#11210,#2762);
#2216=LINE('',#11213,#2763);
#2217=LINE('',#11215,#2764);
#2218=LINE('',#11216,#2765);
#2219=LINE('',#11219,#2766);
#2220=LINE('',#11221,#2767);
#2221=LINE('',#11222,#2768);
#2222=LINE('',#11224,#2769);
#2223=LINE('',#11225,#2770);
#2224=LINE('',#11232,#2771);
#2225=LINE('',#11249,#2772);
#2226=LINE('',#11300,#2773);
#2227=LINE('',#11304,#2774);
#2228=LINE('',#11306,#2775);
#2229=LINE('',#11308,#2776);
#2230=LINE('',#11309,#2777);
#2231=LINE('',#11312,#2778);
#2232=LINE('',#11314,#2779);
#2233=LINE('',#11315,#2780);
#2234=LINE('',#11318,#2781);
#2235=LINE('',#11320,#2782);
#2236=LINE('',#11321,#2783);
#2237=LINE('',#11332,#2784);
#2238=LINE('',#11338,#2785);
#2239=LINE('',#11344,#2786);
#2240=LINE('',#11350,#2787);
#2241=LINE('',#11363,#2788);
#2242=LINE('',#11366,#2789);
#2243=LINE('',#11369,#2790);
#2244=LINE('',#11375,#2791);
#2245=LINE('',#11377,#2792);
#2246=LINE('',#11379,#2793);
#2247=LINE('',#11381,#2794);
#2248=LINE('',#11383,#2795);
#2249=LINE('',#11385,#2796);
#2250=LINE('',#11387,#2797);
#2251=LINE('',#11388,#2798);
#2252=LINE('',#11391,#2799);
#2253=LINE('',#11393,#2800);
#2254=LINE('',#11394,#2801);
#2255=LINE('',#11397,#2802);
#2256=LINE('',#11398,#2803);
#2257=LINE('',#11401,#2804);
#2258=LINE('',#11402,#2805);
#2259=LINE('',#11405,#2806);
#2260=LINE('',#11406,#2807);
#2261=LINE('',#11409,#2808);
#2262=LINE('',#11411,#2809);
#2263=LINE('',#11413,#2810);
#2264=LINE('',#11414,#2811);
#2265=LINE('',#11416,#2812);
#2266=LINE('',#11418,#2813);
#2267=LINE('',#11420,#2814);
#2268=LINE('',#11426,#2815);
#2269=LINE('',#11428,#2816);
#2270=LINE('',#11430,#2817);
#2271=LINE('',#11431,#2818);
#2272=LINE('',#11434,#2819);
#2273=LINE('',#11436,#2820);
#2274=LINE('',#11437,#2821);
#2275=LINE('',#11440,#2822);
#2276=LINE('',#11442,#2823);
#2277=LINE('',#11443,#2824);
#2278=LINE('',#11446,#2825);
#2279=LINE('',#11448,#2826);
#2280=LINE('',#11449,#2827);
#2281=LINE('',#11452,#2828);
#2282=LINE('',#11454,#2829);
#2283=LINE('',#11455,#2830);
#2284=LINE('',#11457,#2831);
#2285=LINE('',#11458,#2832);
#2286=LINE('',#11466,#2833);
#2287=LINE('',#11470,#2834);
#2288=LINE('',#11474,#2835);
#2289=VECTOR('',#7381,0.25);
#2290=VECTOR('',#7388,0.25);
#2291=VECTOR('',#7395,0.25);
#2292=VECTOR('',#7402,0.25);
#2293=VECTOR('',#7409,0.275);
#2294=VECTOR('',#7416,0.275);
#2295=VECTOR('',#7423,0.275);
#2296=VECTOR('',#7430,0.275);
#2297=VECTOR('',#7437,0.275);
#2298=VECTOR('',#7444,0.275);
#2299=VECTOR('',#7451,0.275);
#2300=VECTOR('',#7458,0.275);
#2301=VECTOR('',#7463,1.);
#2302=VECTOR('',#7464,1.);
#2303=VECTOR('',#7465,1.);
#2304=VECTOR('',#7466,1.);
#2305=VECTOR('',#7469,1.);
#2306=VECTOR('',#7470,1.);
#2307=VECTOR('',#7471,1.);
#2308=VECTOR('',#7474,1.);
#2309=VECTOR('',#7475,1.);
#2310=VECTOR('',#7476,1.);
#2311=VECTOR('',#7479,1.);
#2312=VECTOR('',#7480,1.);
#2313=VECTOR('',#7489,1.);
#2314=VECTOR('',#7490,1.);
#2315=VECTOR('',#7491,1.);
#2316=VECTOR('',#7492,1.);
#2317=VECTOR('',#7495,1.);
#2318=VECTOR('',#7496,1.);
#2319=VECTOR('',#7497,1.);
#2320=VECTOR('',#7500,1.);
#2321=VECTOR('',#7501,1.);
#2322=VECTOR('',#7502,1.);
#2323=VECTOR('',#7505,1.);
#2324=VECTOR('',#7506,1.);
#2325=VECTOR('',#7515,1.);
#2326=VECTOR('',#7516,1.);
#2327=VECTOR('',#7517,1.);
#2328=VECTOR('',#7518,1.);
#2329=VECTOR('',#7521,1.);
#2330=VECTOR('',#7522,1.);
#2331=VECTOR('',#7523,1.);
#2332=VECTOR('',#7526,1.);
#2333=VECTOR('',#7527,1.);
#2334=VECTOR('',#7528,1.);
#2335=VECTOR('',#7531,1.);
#2336=VECTOR('',#7532,1.);
#2337=VECTOR('',#7541,1.);
#2338=VECTOR('',#7542,1.);
#2339=VECTOR('',#7543,1.);
#2340=VECTOR('',#7544,1.);
#2341=VECTOR('',#7547,1.);
#2342=VECTOR('',#7548,1.);
#2343=VECTOR('',#7549,1.);
#2344=VECTOR('',#7552,1.);
#2345=VECTOR('',#7553,1.);
#2346=VECTOR('',#7554,1.);
#2347=VECTOR('',#7557,1.);
#2348=VECTOR('',#7558,1.);
#2349=VECTOR('',#7567,1.);
#2350=VECTOR('',#7568,1.);
#2351=VECTOR('',#7569,1.);
#2352=VECTOR('',#7570,1.);
#2353=VECTOR('',#7573,1.);
#2354=VECTOR('',#7574,1.);
#2355=VECTOR('',#7575,1.);
#2356=VECTOR('',#7578,1.);
#2357=VECTOR('',#7579,1.);
#2358=VECTOR('',#7580,1.);
#2359=VECTOR('',#7583,1.);
#2360=VECTOR('',#7584,1.);
#2361=VECTOR('',#7595,0.33);
#2362=VECTOR('',#7602,0.33);
#2363=VECTOR('',#7609,0.44);
#2364=VECTOR('',#7616,0.44);
#2365=VECTOR('',#7623,0.44);
#2366=VECTOR('',#7630,0.44);
#2367=VECTOR('',#7637,3.1);
#2368=VECTOR('',#7642,1.);
#2369=VECTOR('',#7643,1.);
#2370=VECTOR('',#7644,1.);
#2371=VECTOR('',#7645,1.);
#2372=VECTOR('',#7648,1.);
#2373=VECTOR('',#7649,1.);
#2374=VECTOR('',#7650,1.);
#2375=VECTOR('',#7653,1.);
#2376=VECTOR('',#7654,1.);
#2377=VECTOR('',#7655,1.);
#2378=VECTOR('',#7656,1.);
#2379=VECTOR('',#7659,1.);
#2380=VECTOR('',#7660,1.);
#2381=VECTOR('',#7661,1.);
#2382=VECTOR('',#7664,1.);
#2383=VECTOR('',#7665,1.);
#2384=VECTOR('',#7666,1.);
#2385=VECTOR('',#7669,1.);
#2386=VECTOR('',#7680,0.425);
#2387=VECTOR('',#7687,0.595);
#2388=VECTOR('',#7700,0.425);
#2389=VECTOR('',#7707,0.595);
#2390=VECTOR('',#7720,0.425);
#2391=VECTOR('',#7727,0.595);
#2392=VECTOR('',#7740,0.425);
#2393=VECTOR('',#7747,0.595);
#2394=VECTOR('',#7760,0.33);
#2395=VECTOR('',#7767,0.33);
#2396=VECTOR('',#7774,0.44);
#2397=VECTOR('',#7781,0.44);
#2398=VECTOR('',#7788,0.44);
#2399=VECTOR('',#7795,0.44);
#2400=VECTOR('',#7802,3.1);
#2401=VECTOR('',#7807,1.);
#2402=VECTOR('',#7808,1.);
#2403=VECTOR('',#7809,1.);
#2404=VECTOR('',#7810,1.);
#2405=VECTOR('',#7813,1.);
#2406=VECTOR('',#7814,1.);
#2407=VECTOR('',#7815,1.);
#2408=VECTOR('',#7818,1.);
#2409=VECTOR('',#7819,1.);
#2410=VECTOR('',#7820,1.);
#2411=VECTOR('',#7821,1.);
#2412=VECTOR('',#7824,1.);
#2413=VECTOR('',#7825,1.);
#2414=VECTOR('',#7826,1.);
#2415=VECTOR('',#7829,1.);
#2416=VECTOR('',#7830,1.);
#2417=VECTOR('',#7831,1.);
#2418=VECTOR('',#7834,1.);
#2419=VECTOR('',#7845,0.425);
#2420=VECTOR('',#7852,0.595);
#2421=VECTOR('',#7865,0.425);
#2422=VECTOR('',#7872,0.595);
#2423=VECTOR('',#7885,0.425);
#2424=VECTOR('',#7892,0.595);
#2425=VECTOR('',#7905,0.425);
#2426=VECTOR('',#7912,0.595);
#2427=VECTOR('',#7923,1.);
#2428=VECTOR('',#7924,1.);
#2429=VECTOR('',#7925,1.);
#2430=VECTOR('',#7926,1.);
#2431=VECTOR('',#7929,1.);
#2432=VECTOR('',#7930,1.);
#2433=VECTOR('',#7931,1.);
#2434=VECTOR('',#7934,1.);
#2435=VECTOR('',#7935,1.);
#2436=VECTOR('',#7936,1.);
#2437=VECTOR('',#7939,1.);
#2438=VECTOR('',#7940,1.);
#2439=VECTOR('',#7941,1.);
#2440=VECTOR('',#7944,1.);
#2441=VECTOR('',#7945,1.);
#2442=VECTOR('',#7946,1.);
#2443=VECTOR('',#7949,1.);
#2444=VECTOR('',#7950,1.);
#2445=VECTOR('',#7951,1.);
#2446=VECTOR('',#7954,1.);
#2447=VECTOR('',#7955,1.);
#2448=VECTOR('',#7956,1.);
#2449=VECTOR('',#7959,1.);
#2450=VECTOR('',#7960,1.);
#2451=VECTOR('',#7961,1.);
#2452=VECTOR('',#7964,1.);
#2453=VECTOR('',#7965,1.);
#2454=VECTOR('',#7966,1.);
#2455=VECTOR('',#7969,1.);
#2456=VECTOR('',#7970,1.);
#2457=VECTOR('',#7971,1.);
#2458=VECTOR('',#7972,1.);
#2459=VECTOR('',#7975,1.);
#2460=VECTOR('',#7976,1.);
#2461=VECTOR('',#7977,1.);
#2462=VECTOR('',#7980,1.);
#2463=VECTOR('',#7981,1.);
#2464=VECTOR('',#7982,1.);
#2465=VECTOR('',#7985,1.);
#2466=VECTOR('',#7986,1.);
#2467=VECTOR('',#7987,1.);
#2468=VECTOR('',#7990,1.);
#2469=VECTOR('',#7991,1.);
#2470=VECTOR('',#7992,1.);
#2471=VECTOR('',#7995,1.);
#2472=VECTOR('',#7996,1.);
#2473=VECTOR('',#7997,1.);
#2474=VECTOR('',#8000,1.);
#2475=VECTOR('',#8001,1.);
#2476=VECTOR('',#8002,1.);
#2477=VECTOR('',#8005,1.);
#2478=VECTOR('',#8006,1.);
#2479=VECTOR('',#8007,1.);
#2480=VECTOR('',#8010,1.);
#2481=VECTOR('',#8011,1.);
#2482=VECTOR('',#8012,1.);
#2483=VECTOR('',#8015,1.);
#2484=VECTOR('',#8016,1.);
#2485=VECTOR('',#8017,1.);
#2486=VECTOR('',#8018,1.);
#2487=VECTOR('',#8021,1.);
#2488=VECTOR('',#8022,1.);
#2489=VECTOR('',#8023,1.);
#2490=VECTOR('',#8026,1.);
#2491=VECTOR('',#8027,1.);
#2492=VECTOR('',#8028,1.);
#2493=VECTOR('',#8031,1.);
#2494=VECTOR('',#8032,1.);
#2495=VECTOR('',#8033,1.);
#2496=VECTOR('',#8036,1.);
#2497=VECTOR('',#8037,1.);
#2498=VECTOR('',#8038,1.);
#2499=VECTOR('',#8041,1.);
#2500=VECTOR('',#8042,1.);
#2501=VECTOR('',#8043,1.);
#2502=VECTOR('',#8046,1.);
#2503=VECTOR('',#8047,1.);
#2504=VECTOR('',#8048,1.);
#2505=VECTOR('',#8051,1.);
#2506=VECTOR('',#8052,1.);
#2507=VECTOR('',#8053,1.);
#2508=VECTOR('',#8056,1.);
#2509=VECTOR('',#8057,1.);
#2510=VECTOR('',#8058,1.);
#2511=VECTOR('',#8061,1.);
#2512=VECTOR('',#8062,1.);
#2513=VECTOR('',#8063,1.);
#2514=VECTOR('',#8064,1.);
#2515=VECTOR('',#8067,1.);
#2516=VECTOR('',#8068,1.);
#2517=VECTOR('',#8069,1.);
#2518=VECTOR('',#8072,1.);
#2519=VECTOR('',#8073,1.);
#2520=VECTOR('',#8074,1.);
#2521=VECTOR('',#8077,1.);
#2522=VECTOR('',#8078,1.);
#2523=VECTOR('',#8079,1.);
#2524=VECTOR('',#8082,1.);
#2525=VECTOR('',#8083,1.);
#2526=VECTOR('',#8084,1.);
#2527=VECTOR('',#8087,1.);
#2528=VECTOR('',#8088,1.);
#2529=VECTOR('',#8089,1.);
#2530=VECTOR('',#8092,1.);
#2531=VECTOR('',#8093,1.);
#2532=VECTOR('',#8094,1.);
#2533=VECTOR('',#8097,1.);
#2534=VECTOR('',#8098,1.);
#2535=VECTOR('',#8099,1.);
#2536=VECTOR('',#8102,1.);
#2537=VECTOR('',#8103,1.);
#2538=VECTOR('',#8104,1.);
#2539=VECTOR('',#8109,0.21);
#2540=VECTOR('',#8114,1.);
#2541=VECTOR('',#8115,1.);
#2542=VECTOR('',#8116,1.);
#2543=VECTOR('',#8119,1.);
#2544=VECTOR('',#8120,1.);
#2545=VECTOR('',#8121,1.);
#2546=VECTOR('',#8124,1.);
#2547=VECTOR('',#8125,1.);
#2548=VECTOR('',#8128,1.);
#2549=VECTOR('',#8129,1.);
#2550=VECTOR('',#8130,1.);
#2551=VECTOR('',#8133,1.);
#2552=VECTOR('',#8134,1.);
#2553=VECTOR('',#8137,1.);
#2554=VECTOR('',#8138,1.);
#2555=VECTOR('',#8139,1.);
#2556=VECTOR('',#8142,1.);
#2557=VECTOR('',#8143,1.);
#2558=VECTOR('',#8146,1.);
#2559=VECTOR('',#8147,1.);
#2560=VECTOR('',#8156,1.);
#2561=VECTOR('',#8157,1.);
#2562=VECTOR('',#8158,1.);
#2563=VECTOR('',#8159,1.);
#2564=VECTOR('',#8162,1.);
#2565=VECTOR('',#8163,1.);
#2566=VECTOR('',#8164,1.);
#2567=VECTOR('',#8167,1.);
#2568=VECTOR('',#8168,1.);
#2569=VECTOR('',#8169,1.);
#2570=VECTOR('',#8174,1.);
#2571=VECTOR('',#8175,1.);
#2572=VECTOR('',#8176,1.);
#2573=VECTOR('',#8177,1.);
#2574=VECTOR('',#8178,1.);
#2575=VECTOR('',#8179,1.);
#2576=VECTOR('',#8180,1.);
#2577=VECTOR('',#8183,1.);
#2578=VECTOR('',#8184,1.);
#2579=VECTOR('',#8187,1.);
#2580=VECTOR('',#8188,1.);
#2581=VECTOR('',#8191,1.);
#2582=VECTOR('',#8192,1.);
#2583=VECTOR('',#8193,1.);
#2584=VECTOR('',#8194,1.);
#2585=VECTOR('',#8195,1.);
#2586=VECTOR('',#8198,1.);
#2587=VECTOR('',#8201,1.);
#2588=VECTOR('',#8204,1.);
#2589=VECTOR('',#8209,0.21);
#2590=VECTOR('',#8218,1.);
#2591=VECTOR('',#8221,1.);
#2592=VECTOR('',#8224,1.);
#2593=VECTOR('',#8231,1.);
#2594=VECTOR('',#8232,1.);
#2595=VECTOR('',#8233,1.);
#2596=VECTOR('',#8234,1.);
#2597=VECTOR('',#8237,1.);
#2598=VECTOR('',#8238,1.);
#2599=VECTOR('',#8239,1.);
#2600=VECTOR('',#8242,1.);
#2601=VECTOR('',#8243,1.);
#2602=VECTOR('',#8244,1.);
#2603=VECTOR('',#8247,1.);
#2604=VECTOR('',#8248,1.);
#2605=VECTOR('',#8249,1.);
#2606=VECTOR('',#8252,1.);
#2607=VECTOR('',#8253,1.);
#2608=VECTOR('',#8254,1.);
#2609=VECTOR('',#8257,1.);
#2610=VECTOR('',#8258,1.);
#2611=VECTOR('',#8275,0.4);
#2612=VECTOR('',#8280,0.425);
#2613=VECTOR('',#8285,0.41);
#2614=VECTOR('',#8294,0.26);
#2615=VECTOR('',#8297,0.25);
#2616=VECTOR('',#8302,1.);
#2617=VECTOR('',#8303,1.);
#2618=VECTOR('',#8304,1.);
#2619=VECTOR('',#8305,1.);
#2620=VECTOR('',#8308,1.);
#2621=VECTOR('',#8309,1.);
#2622=VECTOR('',#8310,1.);
#2623=VECTOR('',#8313,1.);
#2624=VECTOR('',#8314,1.);
#2625=VECTOR('',#8315,1.);
#2626=VECTOR('',#8318,1.);
#2627=VECTOR('',#8319,1.);
#2628=VECTOR('',#8320,1.);
#2629=VECTOR('',#8323,1.);
#2630=VECTOR('',#8324,1.);
#2631=VECTOR('',#8325,1.);
#2632=VECTOR('',#8328,1.);
#2633=VECTOR('',#8329,1.);
#2634=VECTOR('',#8346,0.475);
#2635=VECTOR('',#8351,0.5);
#2636=VECTOR('',#8356,0.485);
#2637=VECTOR('',#8365,0.31);
#2638=VECTOR('',#8368,0.3);
#2639=VECTOR('',#8377,2.05);
#2640=VECTOR('',#8384,2.05);
#2641=VECTOR('',#8395,3.);
#2642=VECTOR('',#8402,3.);
#2643=VECTOR('',#8413,0.6);
#2644=VECTOR('',#8420,0.6);
#2645=VECTOR('',#8427,0.6);
#2646=VECTOR('',#8434,0.6);
#2647=VECTOR('',#8439,1.);
#2648=VECTOR('',#8440,1.);
#2649=VECTOR('',#8441,1.);
#2650=VECTOR('',#8442,1.);
#2651=VECTOR('',#8445,1.);
#2652=VECTOR('',#8446,1.);
#2653=VECTOR('',#8447,1.);
#2654=VECTOR('',#8450,1.);
#2655=VECTOR('',#8451,1.);
#2656=VECTOR('',#8452,1.);
#2657=VECTOR('',#8455,1.);
#2658=VECTOR('',#8456,1.);
#2659=VECTOR('',#8457,1.);
#2660=VECTOR('',#8460,1.);
#2661=VECTOR('',#8461,1.);
#2662=VECTOR('',#8462,1.);
#2663=VECTOR('',#8465,1.);
#2664=VECTOR('',#8466,1.);
#2665=VECTOR('',#8467,1.);
#2666=VECTOR('',#8470,1.);
#2667=VECTOR('',#8471,1.);
#2668=VECTOR('',#8472,1.);
#2669=VECTOR('',#8475,1.);
#2670=VECTOR('',#8476,1.);
#2671=VECTOR('',#8487,1.8);
#2672=VECTOR('',#8504,0.25);
#2673=VECTOR('',#8507,0.25);
#2674=VECTOR('',#8512,1.65);
#2675=VECTOR('',#8517,0.25);
#2676=VECTOR('',#8520,0.25);
#2677=VECTOR('',#8523,0.25);
#2678=VECTOR('',#8526,0.25);
#2679=VECTOR('',#8539,1.75);
#2680=VECTOR('',#8546,0.6);
#2681=VECTOR('',#8561,0.625);
#2682=VECTOR('',#8566,0.65);
#2683=VECTOR('',#8571,0.635);
#2684=VECTOR('',#8580,0.41);
#2685=VECTOR('',#8585,0.4);
#2686=VECTOR('',#8590,0.36);
#2687=VECTOR('',#8595,1.);
#2688=VECTOR('',#8596,1.);
#2689=VECTOR('',#8597,1.);
#2690=VECTOR('',#8598,1.);
#2691=VECTOR('',#8601,1.);
#2692=VECTOR('',#8602,1.);
#2693=VECTOR('',#8603,1.);
#2694=VECTOR('',#8606,1.);
#2695=VECTOR('',#8607,1.);
#2696=VECTOR('',#8608,1.);
#2697=VECTOR('',#8611,1.);
#2698=VECTOR('',#8612,1.);
#2699=VECTOR('',#8613,1.);
#2700=VECTOR('',#8616,1.);
#2701=VECTOR('',#8617,1.);
#2702=VECTOR('',#8618,1.);
#2703=VECTOR('',#8621,1.);
#2704=VECTOR('',#8622,1.);
#2705=VECTOR('',#8633,0.42);
#2706=VECTOR('',#8640,0.8);
#2707=VECTOR('',#8651,0.734027674973257);
#2708=VECTOR('',#8658,0.734027674973257);
#2709=VECTOR('',#8661,1.);
#2710=VECTOR('',#8662,1.);
#2711=VECTOR('',#8665,1.);
#2712=VECTOR('',#8668,1.);
#2713=VECTOR('',#8673,0.4);
#2714=VECTOR('',#8678,1.);
#2715=VECTOR('',#8681,1.);
#2716=VECTOR('',#8840,1.);
#2717=VECTOR('',#8841,1.);
#2718=VECTOR('',#8842,1.);
#2719=VECTOR('',#8843,1.);
#2720=VECTOR('',#8848,1.);
#2721=VECTOR('',#8849,1.);
#2722=VECTOR('',#8852,1.);
#2723=VECTOR('',#8853,1.);
#2724=VECTOR('',#8854,1.);
#2725=VECTOR('',#8857,1.);
#2726=VECTOR('',#8876,1.);
#2727=VECTOR('',#8879,0.6);
#2728=VECTOR('',#8886,0.6);
#2729=VECTOR('',#8897,0.605);
#2730=VECTOR('',#8904,1.);
#2731=VECTOR('',#8917,0.605);
#2732=VECTOR('',#8924,1.);
#2733=VECTOR('',#8937,0.54);
#2734=VECTOR('',#8942,1.);
#2735=VECTOR('',#8943,1.);
#2736=VECTOR('',#8944,1.);
#2737=VECTOR('',#8945,1.);
#2738=VECTOR('',#8948,1.);
#2739=VECTOR('',#8949,1.);
#2740=VECTOR('',#8950,1.);
#2741=VECTOR('',#8953,1.);
#2742=VECTOR('',#8954,1.);
#2743=VECTOR('',#8955,1.);
#2744=VECTOR('',#8958,1.);
#2745=VECTOR('',#8959,1.);
#2746=VECTOR('',#8960,1.);
#2747=VECTOR('',#8963,1.);
#2748=VECTOR('',#8964,1.);
#2749=VECTOR('',#8965,1.);
#2750=VECTOR('',#8968,1.);
#2751=VECTOR('',#8969,1.);
#2752=VECTOR('',#8980,0.54);
#2753=VECTOR('',#8985,1.);
#2754=VECTOR('',#8986,1.);
#2755=VECTOR('',#8987,1.);
#2756=VECTOR('',#8988,1.);
#2757=VECTOR('',#8991,1.);
#2758=VECTOR('',#8992,1.);
#2759=VECTOR('',#8993,1.);
#2760=VECTOR('',#8996,1.);
#2761=VECTOR('',#8997,1.);
#2762=VECTOR('',#8998,1.);
#2763=VECTOR('',#9001,1.);
#2764=VECTOR('',#9002,1.);
#2765=VECTOR('',#9003,1.);
#2766=VECTOR('',#9006,1.);
#2767=VECTOR('',#9007,1.);
#2768=VECTOR('',#9008,1.);
#2769=VECTOR('',#9011,1.);
#2770=VECTOR('',#9012,1.);
#2771=VECTOR('',#9021,1.);
#2772=VECTOR('',#9028,0.21);
#2773=VECTOR('',#9033,1.);
#2774=VECTOR('',#9036,1.);
#2775=VECTOR('',#9037,1.);
#2776=VECTOR('',#9038,1.);
#2777=VECTOR('',#9039,1.);
#2778=VECTOR('',#9042,1.);
#2779=VECTOR('',#9043,1.);
#2780=VECTOR('',#9044,1.);
#2781=VECTOR('',#9047,1.);
#2782=VECTOR('',#9048,1.);
#2783=VECTOR('',#9049,1.);
#2784=VECTOR('',#9064,0.275);
#2785=VECTOR('',#9071,0.275);
#2786=VECTOR('',#9078,0.275);
#2787=VECTOR('',#9085,0.275);
#2788=VECTOR('',#9102,3.);
#2789=VECTOR('',#9105,1.5);
#2790=VECTOR('',#9110,1.5);
#2791=VECTOR('',#9117,1.);
#2792=VECTOR('',#9118,1.);
#2793=VECTOR('',#9119,1.);
#2794=VECTOR('',#9120,1.);
#2795=VECTOR('',#9121,1.);
#2796=VECTOR('',#9122,1.);
#2797=VECTOR('',#9123,1.);
#2798=VECTOR('',#9124,1.);
#2799=VECTOR('',#9127,1.);
#2800=VECTOR('',#9128,1.);
#2801=VECTOR('',#9129,1.);
#2802=VECTOR('',#9132,1.);
#2803=VECTOR('',#9133,1.);
#2804=VECTOR('',#9136,1.);
#2805=VECTOR('',#9137,1.);
#2806=VECTOR('',#9140,1.);
#2807=VECTOR('',#9141,1.);
#2808=VECTOR('',#9144,1.);
#2809=VECTOR('',#9145,1.);
#2810=VECTOR('',#9146,1.);
#2811=VECTOR('',#9147,1.);
#2812=VECTOR('',#9150,1.);
#2813=VECTOR('',#9153,1.);
#2814=VECTOR('',#9156,1.);
#2815=VECTOR('',#9163,1.);
#2816=VECTOR('',#9164,1.);
#2817=VECTOR('',#9165,1.);
#2818=VECTOR('',#9166,1.);
#2819=VECTOR('',#9169,1.);
#2820=VECTOR('',#9170,1.);
#2821=VECTOR('',#9171,1.);
#2822=VECTOR('',#9174,1.);
#2823=VECTOR('',#9175,1.);
#2824=VECTOR('',#9176,1.);
#2825=VECTOR('',#9179,1.);
#2826=VECTOR('',#9180,1.);
#2827=VECTOR('',#9181,1.);
#2828=VECTOR('',#9184,1.);
#2829=VECTOR('',#9185,1.);
#2830=VECTOR('',#9186,1.);
#2831=VECTOR('',#9189,1.);
#2832=VECTOR('',#9190,1.);
#2833=VECTOR('',#9201,0.235);
#2834=VECTOR('',#9206,0.25);
#2835=VECTOR('',#9211,0.2125);
#2836=CIRCLE('',#6717,0.25);
#2837=CIRCLE('',#6718,0.25);
#2838=CIRCLE('',#6720,0.25);
#2839=CIRCLE('',#6721,0.25);
#2840=CIRCLE('',#6723,0.25);
#2841=CIRCLE('',#6724,0.25);
#2842=CIRCLE('',#6726,0.25);
#2843=CIRCLE('',#6727,0.25);
#2844=CIRCLE('',#6729,0.275);
#2845=CIRCLE('',#6730,0.275);
#2846=CIRCLE('',#6732,0.275);
#2847=CIRCLE('',#6733,0.275);
#2848=CIRCLE('',#6735,0.275);
#2849=CIRCLE('',#6736,0.275);
#2850=CIRCLE('',#6738,0.275);
#2851=CIRCLE('',#6739,0.275);
#2852=CIRCLE('',#6741,0.275);
#2853=CIRCLE('',#6742,0.275);
#2854=CIRCLE('',#6744,0.275);
#2855=CIRCLE('',#6745,0.275);
#2856=CIRCLE('',#6747,0.275);
#2857=CIRCLE('',#6748,0.275);
#2858=CIRCLE('',#6750,0.275);
#2859=CIRCLE('',#6751,0.275);
#2860=CIRCLE('',#6788,0.33);
#2861=CIRCLE('',#6789,0.33);
#2862=CIRCLE('',#6791,0.33);
#2863=CIRCLE('',#6792,0.33);
#2864=CIRCLE('',#6794,0.44);
#2865=CIRCLE('',#6795,0.44);
#2866=CIRCLE('',#6797,0.44);
#2867=CIRCLE('',#6798,0.44);
#2868=CIRCLE('',#6800,0.44);
#2869=CIRCLE('',#6801,0.44);
#2870=CIRCLE('',#6803,0.44);
#2871=CIRCLE('',#6804,0.44);
#2872=CIRCLE('',#6806,3.1);
#2873=CIRCLE('',#6807,3.1);
#2874=CIRCLE('',#6818,0.425);
#2875=CIRCLE('',#6819,0.425);
#2876=CIRCLE('',#6821,0.595);
#2877=CIRCLE('',#6822,0.595);
#2878=CIRCLE('',#6827,0.425);
#2879=CIRCLE('',#6828,0.425);
#2880=CIRCLE('',#6830,0.595);
#2881=CIRCLE('',#6831,0.595);
#2882=CIRCLE('',#6836,0.425);
#2883=CIRCLE('',#6837,0.425);
#2884=CIRCLE('',#6839,0.595);
#2885=CIRCLE('',#6840,0.595);
#2886=CIRCLE('',#6845,0.425);
#2887=CIRCLE('',#6846,0.425);
#2888=CIRCLE('',#6848,0.595);
#2889=CIRCLE('',#6849,0.595);
#2890=CIRCLE('',#6854,0.33);
#2891=CIRCLE('',#6855,0.33);
#2892=CIRCLE('',#6857,0.33);
#2893=CIRCLE('',#6858,0.33);
#2894=CIRCLE('',#6860,0.44);
#2895=CIRCLE('',#6861,0.44);
#2896=CIRCLE('',#6863,0.44);
#2897=CIRCLE('',#6864,0.44);
#2898=CIRCLE('',#6866,0.44);
#2899=CIRCLE('',#6867,0.44);
#2900=CIRCLE('',#6869,0.44);
#2901=CIRCLE('',#6870,0.44);
#2902=CIRCLE('',#6872,3.1);
#2903=CIRCLE('',#6873,3.1);
#2904=CIRCLE('',#6884,0.425);
#2905=CIRCLE('',#6885,0.425);
#2906=CIRCLE('',#6887,0.595);
#2907=CIRCLE('',#6888,0.595);
#2908=CIRCLE('',#6893,0.425);
#2909=CIRCLE('',#6894,0.425);
#2910=CIRCLE('',#6896,0.595);
#2911=CIRCLE('',#6897,0.595);
#2912=CIRCLE('',#6902,0.425);
#2913=CIRCLE('',#6903,0.425);
#2914=CIRCLE('',#6905,0.595);
#2915=CIRCLE('',#6906,0.595);
#2916=CIRCLE('',#6911,0.425);
#2917=CIRCLE('',#6912,0.425);
#2918=CIRCLE('',#6914,0.595);
#2919=CIRCLE('',#6915,0.595);
#2920=CIRCLE('',#6956,0.21);
#2921=CIRCLE('',#6957,0.21);
#2922=CIRCLE('',#6972,0.2117);
#2923=CIRCLE('',#6981,0.2117);
#2924=CIRCLE('',#6982,0.2117);
#2925=CIRCLE('',#6984,0.2117);
#2926=CIRCLE('',#6999,0.24505);
#2927=CIRCLE('',#7001,0.375);
#2928=CIRCLE('',#7003,0.425);
#2929=CIRCLE('',#7005,0.425);
#2930=CIRCLE('',#7007,0.395);
#2931=CIRCLE('',#7009,0.27);
#2932=CIRCLE('',#7011,0.24505);
#2933=CIRCLE('',#7023,0.2942);
#2934=CIRCLE('',#7025,0.45);
#2935=CIRCLE('',#7027,0.5);
#2936=CIRCLE('',#7029,0.5);
#2937=CIRCLE('',#7031,0.47);
#2938=CIRCLE('',#7033,0.32);
#2939=CIRCLE('',#7035,0.2942);
#2940=CIRCLE('',#7040,2.05);
#2941=CIRCLE('',#7041,2.05);
#2942=CIRCLE('',#7043,2.05);
#2943=CIRCLE('',#7044,2.05);
#2944=CIRCLE('',#7046,2.35);
#2945=CIRCLE('',#7048,3.);
#2946=CIRCLE('',#7049,3.);
#2947=CIRCLE('',#7051,3.);
#2948=CIRCLE('',#7052,3.);
#2949=CIRCLE('',#7056,0.6);
#2950=CIRCLE('',#7057,0.6);
#2951=CIRCLE('',#7059,0.6);
#2952=CIRCLE('',#7060,0.6);
#2953=CIRCLE('',#7062,0.6);
#2954=CIRCLE('',#7063,0.6);
#2955=CIRCLE('',#7065,0.6);
#2956=CIRCLE('',#7066,0.6);
#2957=CIRCLE('',#7079,1.8);
#2958=CIRCLE('',#7080,1.8);
#2959=CIRCLE('',#7082,2.19089023002066);
#2960=CIRCLE('',#7084,2.35);
#2961=CIRCLE('',#7085,2.19089023002066);
#2962=CIRCLE('',#7090,1.65);
#2963=CIRCLE('',#7091,1.65);
#2964=CIRCLE('',#7097,0.6);
#2965=CIRCLE('',#7099,1.75);
#2966=CIRCLE('',#7101,1.75);
#2967=CIRCLE('',#7103,0.6);
#2968=CIRCLE('',#7109,0.6);
#2969=CIRCLE('',#7111,0.65);
#2970=CIRCLE('',#7113,0.65);
#2971=CIRCLE('',#7115,0.62);
#2972=CIRCLE('',#7117,0.42);
#2973=CIRCLE('',#7119,0.3933);
#2974=CIRCLE('',#7121,0.3933);
#2975=CIRCLE('',#7123,0.32);
#2976=CIRCLE('',#7135,0.42);
#2977=CIRCLE('',#7136,0.42);
#2978=CIRCLE('',#7138,0.8);
#2979=CIRCLE('',#7139,0.8);
#2980=CIRCLE('',#7144,0.6175);
#2981=CIRCLE('',#7146,0.6175);
#2982=CIRCLE('',#7151,0.338975);
#2983=CIRCLE('',#7152,0.338975);
#2984=CIRCLE('',#7235,0.6);
#2985=CIRCLE('',#7239,0.6);
#2986=CIRCLE('',#7241,1.);
#2987=CIRCLE('',#7242,0.6);
#2988=CIRCLE('',#7244,1.);
#2989=CIRCLE('',#7245,0.6);
#2990=CIRCLE('',#7248,0.6);
#2991=CIRCLE('',#7250,0.6);
#2992=CIRCLE('',#7255,0.605);
#2993=CIRCLE('',#7256,0.605);
#2994=CIRCLE('',#7258,1.);
#2995=CIRCLE('',#7259,1.);
#2996=CIRCLE('',#7264,0.605);
#2997=CIRCLE('',#7265,0.605);
#2998=CIRCLE('',#7267,1.);
#2999=CIRCLE('',#7268,1.);
#3000=CIRCLE('',#7273,0.54);
#3001=CIRCLE('',#7274,0.54);
#3002=CIRCLE('',#7285,0.54);
#3003=CIRCLE('',#7286,0.54);
#3004=CIRCLE('',#7297,0.21);
#3005=CIRCLE('',#7299,0.21);
#3006=CIRCLE('',#7300,0.21);
#3007=CIRCLE('',#7306,1.5);
#3008=CIRCLE('',#7307,0.6);
#3009=CIRCLE('',#7309,0.6);
#3010=CIRCLE('',#7311,0.275);
#3011=CIRCLE('',#7312,0.275);
#3012=CIRCLE('',#7314,0.275);
#3013=CIRCLE('',#7315,0.275);
#3014=CIRCLE('',#7317,0.275);
#3015=CIRCLE('',#7318,0.275);
#3016=CIRCLE('',#7320,0.275);
#3017=CIRCLE('',#7321,0.275);
#3018=CIRCLE('',#7323,3.);
#3019=CIRCLE('',#7324,1.5);
#3020=CIRCLE('',#7326,3.);
#3021=CIRCLE('',#7327,1.5);
#3022=CIRCLE('',#7330,1.5);
#3023=CIRCLE('',#7353,0.22);
#3024=CIRCLE('',#7355,0.24505);
#3025=CIRCLE('',#7357,0.24505);
#3026=CIRCLE('',#7359,0.175);
#3027=VERTEX_POINT('',#9238);
#3028=VERTEX_POINT('',#9240);
#3029=VERTEX_POINT('',#9244);
#3030=VERTEX_POINT('',#9246);
#3031=VERTEX_POINT('',#9250);
#3032=VERTEX_POINT('',#9252);
#3033=VERTEX_POINT('',#9256);
#3034=VERTEX_POINT('',#9258);
#3035=VERTEX_POINT('',#9262);
#3036=VERTEX_POINT('',#9264);
#3037=VERTEX_POINT('',#9268);
#3038=VERTEX_POINT('',#9270);
#3039=VERTEX_POINT('',#9274);
#3040=VERTEX_POINT('',#9276);
#3041=VERTEX_POINT('',#9280);
#3042=VERTEX_POINT('',#9282);
#3043=VERTEX_POINT('',#9286);
#3044=VERTEX_POINT('',#9288);
#3045=VERTEX_POINT('',#9292);
#3046=VERTEX_POINT('',#9294);
#3047=VERTEX_POINT('',#9298);
#3048=VERTEX_POINT('',#9300);
#3049=VERTEX_POINT('',#9304);
#3050=VERTEX_POINT('',#9306);
#3051=VERTEX_POINT('',#9310);
#3052=VERTEX_POINT('',#9311);
#3053=VERTEX_POINT('',#9313);
#3054=VERTEX_POINT('',#9315);
#3055=VERTEX_POINT('',#9319);
#3056=VERTEX_POINT('',#9321);
#3057=VERTEX_POINT('',#9325);
#3058=VERTEX_POINT('',#9327);
#3059=VERTEX_POINT('',#9337);
#3060=VERTEX_POINT('',#9338);
#3061=VERTEX_POINT('',#9340);
#3062=VERTEX_POINT('',#9342);
#3063=VERTEX_POINT('',#9346);
#3064=VERTEX_POINT('',#9348);
#3065=VERTEX_POINT('',#9352);
#3066=VERTEX_POINT('',#9354);
#3067=VERTEX_POINT('',#9364);
#3068=VERTEX_POINT('',#9365);
#3069=VERTEX_POINT('',#9367);
#3070=VERTEX_POINT('',#9369);
#3071=VERTEX_POINT('',#9373);
#3072=VERTEX_POINT('',#9375);
#3073=VERTEX_POINT('',#9379);
#3074=VERTEX_POINT('',#9381);
#3075=VERTEX_POINT('',#9391);
#3076=VERTEX_POINT('',#9392);
#3077=VERTEX_POINT('',#9394);
#3078=VERTEX_POINT('',#9396);
#3079=VERTEX_POINT('',#9400);
#3080=VERTEX_POINT('',#9402);
#3081=VERTEX_POINT('',#9406);
#3082=VERTEX_POINT('',#9408);
#3083=VERTEX_POINT('',#9418);
#3084=VERTEX_POINT('',#9419);
#3085=VERTEX_POINT('',#9421);
#3086=VERTEX_POINT('',#9423);
#3087=VERTEX_POINT('',#9427);
#3088=VERTEX_POINT('',#9429);
#3089=VERTEX_POINT('',#9433);
#3090=VERTEX_POINT('',#9435);
#3091=VERTEX_POINT('',#9445);
#3092=VERTEX_POINT('',#9447);
#3093=VERTEX_POINT('',#9451);
#3094=VERTEX_POINT('',#9453);
#3095=VERTEX_POINT('',#9457);
#3096=VERTEX_POINT('',#9459);
#3097=VERTEX_POINT('',#9463);
#3098=VERTEX_POINT('',#9465);
#3099=VERTEX_POINT('',#9469);
#3100=VERTEX_POINT('',#9471);
#3101=VERTEX_POINT('',#9475);
#3102=VERTEX_POINT('',#9477);
#3103=VERTEX_POINT('',#9481);
#3104=VERTEX_POINT('',#9483);
#3105=VERTEX_POINT('',#9487);
#3106=VERTEX_POINT('',#9488);
#3107=VERTEX_POINT('',#9490);
#3108=VERTEX_POINT('',#9492);
#3109=VERTEX_POINT('',#9496);
#3110=VERTEX_POINT('',#9498);
#3111=VERTEX_POINT('',#9502);
#3112=VERTEX_POINT('',#9503);
#3113=VERTEX_POINT('',#9505);
#3114=VERTEX_POINT('',#9507);
#3115=VERTEX_POINT('',#9511);
#3116=VERTEX_POINT('',#9516);
#3117=VERTEX_POINT('',#9526);
#3118=VERTEX_POINT('',#9528);
#3119=VERTEX_POINT('',#9532);
#3120=VERTEX_POINT('',#9534);
#3121=VERTEX_POINT('',#9541);
#3122=VERTEX_POINT('',#9543);
#3123=VERTEX_POINT('',#9547);
#3124=VERTEX_POINT('',#9549);
#3125=VERTEX_POINT('',#9556);
#3126=VERTEX_POINT('',#9558);
#3127=VERTEX_POINT('',#9562);
#3128=VERTEX_POINT('',#9564);
#3129=VERTEX_POINT('',#9571);
#3130=VERTEX_POINT('',#9573);
#3131=VERTEX_POINT('',#9577);
#3132=VERTEX_POINT('',#9579);
#3133=VERTEX_POINT('',#9586);
#3134=VERTEX_POINT('',#9588);
#3135=VERTEX_POINT('',#9592);
#3136=VERTEX_POINT('',#9594);
#3137=VERTEX_POINT('',#9598);
#3138=VERTEX_POINT('',#9600);
#3139=VERTEX_POINT('',#9604);
#3140=VERTEX_POINT('',#9606);
#3141=VERTEX_POINT('',#9610);
#3142=VERTEX_POINT('',#9612);
#3143=VERTEX_POINT('',#9616);
#3144=VERTEX_POINT('',#9618);
#3145=VERTEX_POINT('',#9622);
#3146=VERTEX_POINT('',#9624);
#3147=VERTEX_POINT('',#9628);
#3148=VERTEX_POINT('',#9629);
#3149=VERTEX_POINT('',#9631);
#3150=VERTEX_POINT('',#9633);
#3151=VERTEX_POINT('',#9637);
#3152=VERTEX_POINT('',#9639);
#3153=VERTEX_POINT('',#9643);
#3154=VERTEX_POINT('',#9644);
#3155=VERTEX_POINT('',#9646);
#3156=VERTEX_POINT('',#9648);
#3157=VERTEX_POINT('',#9652);
#3158=VERTEX_POINT('',#9657);
#3159=VERTEX_POINT('',#9667);
#3160=VERTEX_POINT('',#9669);
#3161=VERTEX_POINT('',#9673);
#3162=VERTEX_POINT('',#9675);
#3163=VERTEX_POINT('',#9682);
#3164=VERTEX_POINT('',#9684);
#3165=VERTEX_POINT('',#9688);
#3166=VERTEX_POINT('',#9690);
#3167=VERTEX_POINT('',#9697);
#3168=VERTEX_POINT('',#9699);
#3169=VERTEX_POINT('',#9703);
#3170=VERTEX_POINT('',#9705);
#3171=VERTEX_POINT('',#9712);
#3172=VERTEX_POINT('',#9714);
#3173=VERTEX_POINT('',#9718);
#3174=VERTEX_POINT('',#9720);
#3175=VERTEX_POINT('',#9727);
#3176=VERTEX_POINT('',#9728);
#3177=VERTEX_POINT('',#9730);
#3178=VERTEX_POINT('',#9732);
#3179=VERTEX_POINT('',#9736);
#3180=VERTEX_POINT('',#9738);
#3181=VERTEX_POINT('',#9742);
#3182=VERTEX_POINT('',#9744);
#3183=VERTEX_POINT('',#9748);
#3184=VERTEX_POINT('',#9750);
#3185=VERTEX_POINT('',#9754);
#3186=VERTEX_POINT('',#9756);
#3187=VERTEX_POINT('',#9760);
#3188=VERTEX_POINT('',#9762);
#3189=VERTEX_POINT('',#9766);
#3190=VERTEX_POINT('',#9768);
#3191=VERTEX_POINT('',#9772);
#3192=VERTEX_POINT('',#9774);
#3193=VERTEX_POINT('',#9778);
#3194=VERTEX_POINT('',#9780);
#3195=VERTEX_POINT('',#9784);
#3196=VERTEX_POINT('',#9785);
#3197=VERTEX_POINT('',#9787);
#3198=VERTEX_POINT('',#9789);
#3199=VERTEX_POINT('',#9793);
#3200=VERTEX_POINT('',#9795);
#3201=VERTEX_POINT('',#9799);
#3202=VERTEX_POINT('',#9801);
#3203=VERTEX_POINT('',#9805);
#3204=VERTEX_POINT('',#9807);
#3205=VERTEX_POINT('',#9811);
#3206=VERTEX_POINT('',#9813);
#3207=VERTEX_POINT('',#9817);
#3208=VERTEX_POINT('',#9819);
#3209=VERTEX_POINT('',#9823);
#3210=VERTEX_POINT('',#9825);
#3211=VERTEX_POINT('',#9829);
#3212=VERTEX_POINT('',#9831);
#3213=VERTEX_POINT('',#9835);
#3214=VERTEX_POINT('',#9837);
#3215=VERTEX_POINT('',#9841);
#3216=VERTEX_POINT('',#9842);
#3217=VERTEX_POINT('',#9844);
#3218=VERTEX_POINT('',#9846);
#3219=VERTEX_POINT('',#9850);
#3220=VERTEX_POINT('',#9852);
#3221=VERTEX_POINT('',#9856);
#3222=VERTEX_POINT('',#9858);
#3223=VERTEX_POINT('',#9862);
#3224=VERTEX_POINT('',#9864);
#3225=VERTEX_POINT('',#9868);
#3226=VERTEX_POINT('',#9870);
#3227=VERTEX_POINT('',#9874);
#3228=VERTEX_POINT('',#9876);
#3229=VERTEX_POINT('',#9880);
#3230=VERTEX_POINT('',#9882);
#3231=VERTEX_POINT('',#9886);
#3232=VERTEX_POINT('',#9888);
#3233=VERTEX_POINT('',#9892);
#3234=VERTEX_POINT('',#9894);
#3235=VERTEX_POINT('',#9898);
#3236=VERTEX_POINT('',#9899);
#3237=VERTEX_POINT('',#9901);
#3238=VERTEX_POINT('',#9903);
#3239=VERTEX_POINT('',#9907);
#3240=VERTEX_POINT('',#9909);
#3241=VERTEX_POINT('',#9913);
#3242=VERTEX_POINT('',#9915);
#3243=VERTEX_POINT('',#9919);
#3244=VERTEX_POINT('',#9921);
#3245=VERTEX_POINT('',#9925);
#3246=VERTEX_POINT('',#9927);
#3247=VERTEX_POINT('',#9931);
#3248=VERTEX_POINT('',#9933);
#3249=VERTEX_POINT('',#9937);
#3250=VERTEX_POINT('',#9939);
#3251=VERTEX_POINT('',#9943);
#3252=VERTEX_POINT('',#9945);
#3253=VERTEX_POINT('',#9949);
#3254=VERTEX_POINT('',#9951);
#3255=VERTEX_POINT('',#9955);
#3256=VERTEX_POINT('',#9957);
#3257=VERTEX_POINT('',#9961);
#3258=VERTEX_POINT('',#9963);
#3259=VERTEX_POINT('',#9967);
#3260=VERTEX_POINT('',#9969);
#3261=VERTEX_POINT('',#9976);
#3262=VERTEX_POINT('',#9978);
#3263=VERTEX_POINT('',#9985);
#3264=VERTEX_POINT('',#9987);
#3265=VERTEX_POINT('',#10000);
#3266=VERTEX_POINT('',#10001);
#3267=VERTEX_POINT('',#10003);
#3268=VERTEX_POINT('',#10005);
#3269=VERTEX_POINT('',#10009);
#3270=VERTEX_POINT('',#10011);
#3271=VERTEX_POINT('',#10015);
#3272=VERTEX_POINT('',#10017);
#3273=VERTEX_POINT('',#10020);
#3274=VERTEX_POINT('',#10023);
#3275=VERTEX_POINT('',#10025);
#3276=VERTEX_POINT('',#10027);
#3277=VERTEX_POINT('',#10029);
#3278=VERTEX_POINT('',#10031);
#3279=VERTEX_POINT('',#10033);
#3280=VERTEX_POINT('',#10037);
#3281=VERTEX_POINT('',#10041);
#3282=VERTEX_POINT('',#10045);
#3283=VERTEX_POINT('',#10047);
#3284=VERTEX_POINT('',#10049);
#3285=VERTEX_POINT('',#10051);
#3286=VERTEX_POINT('',#10057);
#3287=VERTEX_POINT('',#10059);
#3288=VERTEX_POINT('',#10063);
#3289=VERTEX_POINT('',#10066);
#3290=VERTEX_POINT('',#10068);
#3291=VERTEX_POINT('',#10080);
#3292=VERTEX_POINT('',#10081);
#3293=VERTEX_POINT('',#10083);
#3294=VERTEX_POINT('',#10085);
#3295=VERTEX_POINT('',#10089);
#3296=VERTEX_POINT('',#10091);
#3297=VERTEX_POINT('',#10095);
#3298=VERTEX_POINT('',#10097);
#3299=VERTEX_POINT('',#10101);
#3300=VERTEX_POINT('',#10103);
#3301=VERTEX_POINT('',#10107);
#3302=VERTEX_POINT('',#10109);
#3303=VERTEX_POINT('',#10118);
#3304=VERTEX_POINT('',#10121);
#3305=VERTEX_POINT('',#10124);
#3306=VERTEX_POINT('',#10128);
#3307=VERTEX_POINT('',#10132);
#3308=VERTEX_POINT('',#10136);
#3309=VERTEX_POINT('',#10139);
#3310=VERTEX_POINT('',#10146);
#3311=VERTEX_POINT('',#10147);
#3312=VERTEX_POINT('',#10149);
#3313=VERTEX_POINT('',#10151);
#3314=VERTEX_POINT('',#10155);
#3315=VERTEX_POINT('',#10157);
#3316=VERTEX_POINT('',#10161);
#3317=VERTEX_POINT('',#10163);
#3318=VERTEX_POINT('',#10167);
#3319=VERTEX_POINT('',#10169);
#3320=VERTEX_POINT('',#10173);
#3321=VERTEX_POINT('',#10175);
#3322=VERTEX_POINT('',#10184);
#3323=VERTEX_POINT('',#10187);
#3324=VERTEX_POINT('',#10190);
#3325=VERTEX_POINT('',#10194);
#3326=VERTEX_POINT('',#10198);
#3327=VERTEX_POINT('',#10202);
#3328=VERTEX_POINT('',#10205);
#3329=VERTEX_POINT('',#10213);
#3330=VERTEX_POINT('',#10215);
#3331=VERTEX_POINT('',#10219);
#3332=VERTEX_POINT('',#10221);
#3333=VERTEX_POINT('',#10225);
#3334=VERTEX_POINT('',#10226);
#3335=VERTEX_POINT('',#10229);
#3336=VERTEX_POINT('',#10231);
#3337=VERTEX_POINT('',#10235);
#3338=VERTEX_POINT('',#10237);
#3339=VERTEX_POINT('',#10243);
#3340=VERTEX_POINT('',#10245);
#3341=VERTEX_POINT('',#10249);
#3342=VERTEX_POINT('',#10251);
#3343=VERTEX_POINT('',#10255);
#3344=VERTEX_POINT('',#10257);
#3345=VERTEX_POINT('',#10261);
#3346=VERTEX_POINT('',#10263);
#3347=VERTEX_POINT('',#10267);
#3348=VERTEX_POINT('',#10268);
#3349=VERTEX_POINT('',#10270);
#3350=VERTEX_POINT('',#10272);
#3351=VERTEX_POINT('',#10276);
#3352=VERTEX_POINT('',#10278);
#3353=VERTEX_POINT('',#10282);
#3354=VERTEX_POINT('',#10284);
#3355=VERTEX_POINT('',#10288);
#3356=VERTEX_POINT('',#10290);
#3357=VERTEX_POINT('',#10294);
#3358=VERTEX_POINT('',#10296);
#3359=VERTEX_POINT('',#10300);
#3360=VERTEX_POINT('',#10302);
#3361=VERTEX_POINT('',#10306);
#3362=VERTEX_POINT('',#10308);
#3363=VERTEX_POINT('',#10318);
#3364=VERTEX_POINT('',#10320);
#3365=VERTEX_POINT('',#10324);
#3366=VERTEX_POINT('',#10327);
#3367=VERTEX_POINT('',#10328);
#3368=VERTEX_POINT('',#10330);
#3369=VERTEX_POINT('',#10334);
#3370=VERTEX_POINT('',#10335);
#3371=VERTEX_POINT('',#10346);
#3372=VERTEX_POINT('',#10375);
#3373=VERTEX_POINT('',#10412);
#3374=VERTEX_POINT('',#10447);
#3375=VERTEX_POINT('',#10449);
#3376=VERTEX_POINT('',#10460);
#3377=VERTEX_POINT('',#10490);
#3378=VERTEX_POINT('',#10492);
#3379=VERTEX_POINT('',#10495);
#3380=VERTEX_POINT('',#10496);
#3381=VERTEX_POINT('',#10515);
#3382=VERTEX_POINT('',#10536);
#3383=VERTEX_POINT('',#10537);
#3384=VERTEX_POINT('',#10556);
#3385=VERTEX_POINT('',#10577);
#3386=VERTEX_POINT('',#10578);
#3387=VERTEX_POINT('',#10597);
#3388=VERTEX_POINT('',#10618);
#3389=VERTEX_POINT('',#10619);
#3390=VERTEX_POINT('',#10638);
#3391=VERTEX_POINT('',#10660);
#3392=VERTEX_POINT('',#10697);
#3393=VERTEX_POINT('',#10734);
#3394=VERTEX_POINT('',#10771);
#3395=VERTEX_POINT('',#10808);
#3396=VERTEX_POINT('',#10811);
#3397=VERTEX_POINT('',#10814);
#3398=VERTEX_POINT('',#10818);
#3399=VERTEX_POINT('',#10826);
#3400=VERTEX_POINT('',#10829);
#3401=VERTEX_POINT('',#10833);
#3402=VERTEX_POINT('',#10837);
#3403=VERTEX_POINT('',#10841);
#3404=VERTEX_POINT('',#10844);
#3405=VERTEX_POINT('',#10848);
#3406=VERTEX_POINT('',#10852);
#3407=VERTEX_POINT('',#10857);
#3408=VERTEX_POINT('',#10858);
#3409=VERTEX_POINT('',#10860);
#3410=VERTEX_POINT('',#10862);
#3411=VERTEX_POINT('',#10866);
#3412=VERTEX_POINT('',#10868);
#3413=VERTEX_POINT('',#10872);
#3414=VERTEX_POINT('',#10874);
#3415=VERTEX_POINT('',#10878);
#3416=VERTEX_POINT('',#10880);
#3417=VERTEX_POINT('',#10884);
#3418=VERTEX_POINT('',#10886);
#3419=VERTEX_POINT('',#10896);
#3420=VERTEX_POINT('',#10898);
#3421=VERTEX_POINT('',#10902);
#3422=VERTEX_POINT('',#10904);
#3423=VERTEX_POINT('',#10911);
#3424=VERTEX_POINT('',#10912);
#3425=VERTEX_POINT('',#10916);
#3426=VERTEX_POINT('',#10920);
#3427=VERTEX_POINT('',#10923);
#3428=VERTEX_POINT('',#10927);
#3429=VERTEX_POINT('',#10931);
#3430=VERTEX_POINT('',#10939);
#3431=VERTEX_POINT('',#10941);
#3432=VERTEX_POINT('',#10943);
#3433=VERTEX_POINT('',#10947);
#3434=VERTEX_POINT('',#10951);
#3435=VERTEX_POINT('',#10955);
#3436=VERTEX_POINT('',#10959);
#3437=VERTEX_POINT('',#10974);
#3438=VERTEX_POINT('',#10976);
#3439=VERTEX_POINT('',#11062);
#3440=VERTEX_POINT('',#11063);
#3441=VERTEX_POINT('',#11065);
#3442=VERTEX_POINT('',#11067);
#3443=VERTEX_POINT('',#11071);
#3444=VERTEX_POINT('',#11073);
#3445=VERTEX_POINT('',#11077);
#3446=VERTEX_POINT('',#11079);
#3447=VERTEX_POINT('',#11087);
#3448=VERTEX_POINT('',#11089);
#3449=VERTEX_POINT('',#11092);
#3450=VERTEX_POINT('',#11094);
#3451=VERTEX_POINT('',#11099);
#3452=VERTEX_POINT('',#11103);
#3453=VERTEX_POINT('',#11110);
#3454=VERTEX_POINT('',#11112);
#3455=VERTEX_POINT('',#11116);
#3456=VERTEX_POINT('',#11118);
#3457=VERTEX_POINT('',#11125);
#3458=VERTEX_POINT('',#11127);
#3459=VERTEX_POINT('',#11131);
#3460=VERTEX_POINT('',#11133);
#3461=VERTEX_POINT('',#11140);
#3462=VERTEX_POINT('',#11142);
#3463=VERTEX_POINT('',#11146);
#3464=VERTEX_POINT('',#11147);
#3465=VERTEX_POINT('',#11149);
#3466=VERTEX_POINT('',#11151);
#3467=VERTEX_POINT('',#11155);
#3468=VERTEX_POINT('',#11157);
#3469=VERTEX_POINT('',#11161);
#3470=VERTEX_POINT('',#11163);
#3471=VERTEX_POINT('',#11167);
#3472=VERTEX_POINT('',#11169);
#3473=VERTEX_POINT('',#11173);
#3474=VERTEX_POINT('',#11175);
#3475=VERTEX_POINT('',#11185);
#3476=VERTEX_POINT('',#11187);
#3477=VERTEX_POINT('',#11191);
#3478=VERTEX_POINT('',#11192);
#3479=VERTEX_POINT('',#11194);
#3480=VERTEX_POINT('',#11196);
#3481=VERTEX_POINT('',#11200);
#3482=VERTEX_POINT('',#11202);
#3483=VERTEX_POINT('',#11206);
#3484=VERTEX_POINT('',#11208);
#3485=VERTEX_POINT('',#11212);
#3486=VERTEX_POINT('',#11214);
#3487=VERTEX_POINT('',#11218);
#3488=VERTEX_POINT('',#11220);
#3489=VERTEX_POINT('',#11230);
#3490=VERTEX_POINT('',#11231);
#3491=VERTEX_POINT('',#11235);
#3492=VERTEX_POINT('',#11246);
#3493=VERTEX_POINT('',#11248);
#3494=VERTEX_POINT('',#11250);
#3495=VERTEX_POINT('',#11287);
#3496=VERTEX_POINT('',#11302);
#3497=VERTEX_POINT('',#11303);
#3498=VERTEX_POINT('',#11305);
#3499=VERTEX_POINT('',#11307);
#3500=VERTEX_POINT('',#11311);
#3501=VERTEX_POINT('',#11313);
#3502=VERTEX_POINT('',#11317);
#3503=VERTEX_POINT('',#11319);
#3504=VERTEX_POINT('',#11323);
#3505=VERTEX_POINT('',#11329);
#3506=VERTEX_POINT('',#11331);
#3507=VERTEX_POINT('',#11335);
#3508=VERTEX_POINT('',#11337);
#3509=VERTEX_POINT('',#11341);
#3510=VERTEX_POINT('',#11343);
#3511=VERTEX_POINT('',#11347);
#3512=VERTEX_POINT('',#11349);
#3513=VERTEX_POINT('',#11353);
#3514=VERTEX_POINT('',#11355);
#3515=VERTEX_POINT('',#11358);
#3516=VERTEX_POINT('',#11360);
#3517=VERTEX_POINT('',#11365);
#3518=VERTEX_POINT('',#11373);
#3519=VERTEX_POINT('',#11374);
#3520=VERTEX_POINT('',#11376);
#3521=VERTEX_POINT('',#11378);
#3522=VERTEX_POINT('',#11380);
#3523=VERTEX_POINT('',#11382);
#3524=VERTEX_POINT('',#11384);
#3525=VERTEX_POINT('',#11386);
#3526=VERTEX_POINT('',#11390);
#3527=VERTEX_POINT('',#11392);
#3528=VERTEX_POINT('',#11396);
#3529=VERTEX_POINT('',#11400);
#3530=VERTEX_POINT('',#11404);
#3531=VERTEX_POINT('',#11408);
#3532=VERTEX_POINT('',#11410);
#3533=VERTEX_POINT('',#11412);
#3534=VERTEX_POINT('',#11424);
#3535=VERTEX_POINT('',#11425);
#3536=VERTEX_POINT('',#11427);
#3537=VERTEX_POINT('',#11429);
#3538=VERTEX_POINT('',#11433);
#3539=VERTEX_POINT('',#11435);
#3540=VERTEX_POINT('',#11439);
#3541=VERTEX_POINT('',#11441);
#3542=VERTEX_POINT('',#11445);
#3543=VERTEX_POINT('',#11447);
#3544=VERTEX_POINT('',#11451);
#3545=VERTEX_POINT('',#11453);
#3546=VERTEX_POINT('',#11461);
#3547=VERTEX_POINT('',#11464);
#3548=VERTEX_POINT('',#11468);
#3549=VERTEX_POINT('',#11472);
#3550=EDGE_CURVE('',#3027,#3027,#2836,.T.);
#3551=EDGE_CURVE('',#3027,#3028,#1742,.T.);
#3552=EDGE_CURVE('',#3028,#3028,#2837,.T.);
#3553=EDGE_CURVE('',#3029,#3029,#2838,.T.);
#3554=EDGE_CURVE('',#3029,#3030,#1743,.T.);
#3555=EDGE_CURVE('',#3030,#3030,#2839,.T.);
#3556=EDGE_CURVE('',#3031,#3031,#2840,.T.);
#3557=EDGE_CURVE('',#3031,#3032,#1744,.T.);
#3558=EDGE_CURVE('',#3032,#3032,#2841,.T.);
#3559=EDGE_CURVE('',#3033,#3033,#2842,.T.);
#3560=EDGE_CURVE('',#3033,#3034,#1745,.T.);
#3561=EDGE_CURVE('',#3034,#3034,#2843,.T.);
#3562=EDGE_CURVE('',#3035,#3035,#2844,.T.);
#3563=EDGE_CURVE('',#3035,#3036,#1746,.T.);
#3564=EDGE_CURVE('',#3036,#3036,#2845,.T.);
#3565=EDGE_CURVE('',#3037,#3037,#2846,.T.);
#3566=EDGE_CURVE('',#3037,#3038,#1747,.T.);
#3567=EDGE_CURVE('',#3038,#3038,#2847,.T.);
#3568=EDGE_CURVE('',#3039,#3039,#2848,.T.);
#3569=EDGE_CURVE('',#3039,#3040,#1748,.T.);
#3570=EDGE_CURVE('',#3040,#3040,#2849,.T.);
#3571=EDGE_CURVE('',#3041,#3041,#2850,.T.);
#3572=EDGE_CURVE('',#3041,#3042,#1749,.T.);
#3573=EDGE_CURVE('',#3042,#3042,#2851,.T.);
#3574=EDGE_CURVE('',#3043,#3043,#2852,.T.);
#3575=EDGE_CURVE('',#3043,#3044,#1750,.T.);
#3576=EDGE_CURVE('',#3044,#3044,#2853,.T.);
#3577=EDGE_CURVE('',#3045,#3045,#2854,.T.);
#3578=EDGE_CURVE('',#3045,#3046,#1751,.T.);
#3579=EDGE_CURVE('',#3046,#3046,#2855,.T.);
#3580=EDGE_CURVE('',#3047,#3047,#2856,.T.);
#3581=EDGE_CURVE('',#3047,#3048,#1752,.T.);
#3582=EDGE_CURVE('',#3048,#3048,#2857,.T.);
#3583=EDGE_CURVE('',#3049,#3049,#2858,.T.);
#3584=EDGE_CURVE('',#3049,#3050,#1753,.T.);
#3585=EDGE_CURVE('',#3050,#3050,#2859,.T.);
#3586=EDGE_CURVE('',#3051,#3052,#1754,.T.);
#3587=EDGE_CURVE('',#3052,#3053,#1755,.T.);
#3588=EDGE_CURVE('',#3054,#3053,#1756,.T.);
#3589=EDGE_CURVE('',#3051,#3054,#1757,.T.);
#3590=EDGE_CURVE('',#3055,#3051,#1758,.T.);
#3591=EDGE_CURVE('',#3056,#3054,#1759,.T.);
#3592=EDGE_CURVE('',#3055,#3056,#1760,.T.);
#3593=EDGE_CURVE('',#3057,#3055,#1761,.T.);
#3594=EDGE_CURVE('',#3058,#3056,#1762,.T.);
#3595=EDGE_CURVE('',#3057,#3058,#1763,.T.);
#3596=EDGE_CURVE('',#3052,#3057,#1764,.T.);
#3597=EDGE_CURVE('',#3053,#3058,#1765,.T.);
#3598=EDGE_CURVE('',#3059,#3060,#1766,.T.);
#3599=EDGE_CURVE('',#3060,#3061,#1767,.T.);
#3600=EDGE_CURVE('',#3062,#3061,#1768,.T.);
#3601=EDGE_CURVE('',#3059,#3062,#1769,.T.);
#3602=EDGE_CURVE('',#3063,#3059,#1770,.T.);
#3603=EDGE_CURVE('',#3064,#3062,#1771,.T.);
#3604=EDGE_CURVE('',#3063,#3064,#1772,.T.);
#3605=EDGE_CURVE('',#3065,#3063,#1773,.T.);
#3606=EDGE_CURVE('',#3066,#3064,#1774,.T.);
#3607=EDGE_CURVE('',#3065,#3066,#1775,.T.);
#3608=EDGE_CURVE('',#3060,#3065,#1776,.T.);
#3609=EDGE_CURVE('',#3061,#3066,#1777,.T.);
#3610=EDGE_CURVE('',#3067,#3068,#1778,.T.);
#3611=EDGE_CURVE('',#3068,#3069,#1779,.T.);
#3612=EDGE_CURVE('',#3070,#3069,#1780,.T.);
#3613=EDGE_CURVE('',#3067,#3070,#1781,.T.);
#3614=EDGE_CURVE('',#3071,#3067,#1782,.T.);
#3615=EDGE_CURVE('',#3072,#3070,#1783,.T.);
#3616=EDGE_CURVE('',#3071,#3072,#1784,.T.);
#3617=EDGE_CURVE('',#3073,#3071,#1785,.T.);
#3618=EDGE_CURVE('',#3074,#3072,#1786,.T.);
#3619=EDGE_CURVE('',#3073,#3074,#1787,.T.);
#3620=EDGE_CURVE('',#3068,#3073,#1788,.T.);
#3621=EDGE_CURVE('',#3069,#3074,#1789,.T.);
#3622=EDGE_CURVE('',#3075,#3076,#1790,.T.);
#3623=EDGE_CURVE('',#3076,#3077,#1791,.T.);
#3624=EDGE_CURVE('',#3078,#3077,#1792,.T.);
#3625=EDGE_CURVE('',#3075,#3078,#1793,.T.);
#3626=EDGE_CURVE('',#3079,#3075,#1794,.T.);
#3627=EDGE_CURVE('',#3080,#3078,#1795,.T.);
#3628=EDGE_CURVE('',#3079,#3080,#1796,.T.);
#3629=EDGE_CURVE('',#3081,#3079,#1797,.T.);
#3630=EDGE_CURVE('',#3082,#3080,#1798,.T.);
#3631=EDGE_CURVE('',#3081,#3082,#1799,.T.);
#3632=EDGE_CURVE('',#3076,#3081,#1800,.T.);
#3633=EDGE_CURVE('',#3077,#3082,#1801,.T.);
#3634=EDGE_CURVE('',#3083,#3084,#1802,.T.);
#3635=EDGE_CURVE('',#3084,#3085,#1803,.T.);
#3636=EDGE_CURVE('',#3086,#3085,#1804,.T.);
#3637=EDGE_CURVE('',#3083,#3086,#1805,.T.);
#3638=EDGE_CURVE('',#3087,#3083,#1806,.T.);
#3639=EDGE_CURVE('',#3088,#3086,#1807,.T.);
#3640=EDGE_CURVE('',#3087,#3088,#1808,.T.);
#3641=EDGE_CURVE('',#3089,#3087,#1809,.T.);
#3642=EDGE_CURVE('',#3090,#3088,#1810,.T.);
#3643=EDGE_CURVE('',#3089,#3090,#1811,.T.);
#3644=EDGE_CURVE('',#3084,#3089,#1812,.T.);
#3645=EDGE_CURVE('',#3085,#3090,#1813,.T.);
#3646=EDGE_CURVE('',#3091,#3091,#2860,.T.);
#3647=EDGE_CURVE('',#3091,#3092,#1814,.T.);
#3648=EDGE_CURVE('',#3092,#3092,#2861,.T.);
#3649=EDGE_CURVE('',#3093,#3093,#2862,.T.);
#3650=EDGE_CURVE('',#3093,#3094,#1815,.T.);
#3651=EDGE_CURVE('',#3094,#3094,#2863,.T.);
#3652=EDGE_CURVE('',#3095,#3095,#2864,.T.);
#3653=EDGE_CURVE('',#3095,#3096,#1816,.T.);
#3654=EDGE_CURVE('',#3096,#3096,#2865,.T.);
#3655=EDGE_CURVE('',#3097,#3097,#2866,.T.);
#3656=EDGE_CURVE('',#3097,#3098,#1817,.T.);
#3657=EDGE_CURVE('',#3098,#3098,#2867,.T.);
#3658=EDGE_CURVE('',#3099,#3099,#2868,.T.);
#3659=EDGE_CURVE('',#3099,#3100,#1818,.T.);
#3660=EDGE_CURVE('',#3100,#3100,#2869,.T.);
#3661=EDGE_CURVE('',#3101,#3101,#2870,.T.);
#3662=EDGE_CURVE('',#3101,#3102,#1819,.T.);
#3663=EDGE_CURVE('',#3102,#3102,#2871,.T.);
#3664=EDGE_CURVE('',#3103,#3103,#2872,.T.);
#3665=EDGE_CURVE('',#3103,#3104,#1820,.T.);
#3666=EDGE_CURVE('',#3104,#3104,#2873,.T.);
#3667=EDGE_CURVE('',#3105,#3106,#1821,.T.);
#3668=EDGE_CURVE('',#3107,#3105,#1822,.T.);
#3669=EDGE_CURVE('',#3108,#3107,#1823,.T.);
#3670=EDGE_CURVE('',#3108,#3106,#1824,.T.);
#3671=EDGE_CURVE('',#3107,#3109,#1825,.T.);
#3672=EDGE_CURVE('',#3109,#3110,#1826,.T.);
#3673=EDGE_CURVE('',#3110,#3108,#1827,.T.);
#3674=EDGE_CURVE('',#3111,#3112,#1828,.T.);
#3675=EDGE_CURVE('',#3113,#3112,#1829,.T.);
#3676=EDGE_CURVE('',#3114,#3113,#1830,.T.);
#3677=EDGE_CURVE('',#3114,#3111,#1831,.T.);
#3678=EDGE_CURVE('',#3105,#3115,#1832,.T.);
#3679=EDGE_CURVE('',#3112,#3115,#1833,.T.);
#3680=EDGE_CURVE('',#3111,#3109,#1834,.T.);
#3681=EDGE_CURVE('',#3116,#3113,#1835,.T.);
#3682=EDGE_CURVE('',#3106,#3116,#1836,.T.);
#3683=EDGE_CURVE('',#3110,#3114,#1837,.T.);
#3684=EDGE_CURVE('',#3115,#3116,#1838,.T.);
#3685=EDGE_CURVE('',#3117,#3117,#2874,.T.);
#3686=EDGE_CURVE('',#3117,#3118,#1839,.T.);
#3687=EDGE_CURVE('',#3118,#3118,#2875,.T.);
#3688=EDGE_CURVE('',#3119,#3119,#2876,.T.);
#3689=EDGE_CURVE('',#3119,#3120,#1840,.T.);
#3690=EDGE_CURVE('',#3120,#3120,#2877,.T.);
#3691=EDGE_CURVE('',#3121,#3121,#2878,.T.);
#3692=EDGE_CURVE('',#3121,#3122,#1841,.T.);
#3693=EDGE_CURVE('',#3122,#3122,#2879,.T.);
#3694=EDGE_CURVE('',#3123,#3123,#2880,.T.);
#3695=EDGE_CURVE('',#3123,#3124,#1842,.T.);
#3696=EDGE_CURVE('',#3124,#3124,#2881,.T.);
#3697=EDGE_CURVE('',#3125,#3125,#2882,.T.);
#3698=EDGE_CURVE('',#3125,#3126,#1843,.T.);
#3699=EDGE_CURVE('',#3126,#3126,#2883,.T.);
#3700=EDGE_CURVE('',#3127,#3127,#2884,.T.);
#3701=EDGE_CURVE('',#3127,#3128,#1844,.T.);
#3702=EDGE_CURVE('',#3128,#3128,#2885,.T.);
#3703=EDGE_CURVE('',#3129,#3129,#2886,.T.);
#3704=EDGE_CURVE('',#3129,#3130,#1845,.T.);
#3705=EDGE_CURVE('',#3130,#3130,#2887,.T.);
#3706=EDGE_CURVE('',#3131,#3131,#2888,.T.);
#3707=EDGE_CURVE('',#3131,#3132,#1846,.T.);
#3708=EDGE_CURVE('',#3132,#3132,#2889,.T.);
#3709=EDGE_CURVE('',#3133,#3133,#2890,.T.);
#3710=EDGE_CURVE('',#3133,#3134,#1847,.T.);
#3711=EDGE_CURVE('',#3134,#3134,#2891,.T.);
#3712=EDGE_CURVE('',#3135,#3135,#2892,.T.);
#3713=EDGE_CURVE('',#3135,#3136,#1848,.T.);
#3714=EDGE_CURVE('',#3136,#3136,#2893,.T.);
#3715=EDGE_CURVE('',#3137,#3137,#2894,.T.);
#3716=EDGE_CURVE('',#3137,#3138,#1849,.T.);
#3717=EDGE_CURVE('',#3138,#3138,#2895,.T.);
#3718=EDGE_CURVE('',#3139,#3139,#2896,.T.);
#3719=EDGE_CURVE('',#3139,#3140,#1850,.T.);
#3720=EDGE_CURVE('',#3140,#3140,#2897,.T.);
#3721=EDGE_CURVE('',#3141,#3141,#2898,.T.);
#3722=EDGE_CURVE('',#3141,#3142,#1851,.T.);
#3723=EDGE_CURVE('',#3142,#3142,#2899,.T.);
#3724=EDGE_CURVE('',#3143,#3143,#2900,.T.);
#3725=EDGE_CURVE('',#3143,#3144,#1852,.T.);
#3726=EDGE_CURVE('',#3144,#3144,#2901,.T.);
#3727=EDGE_CURVE('',#3145,#3145,#2902,.T.);
#3728=EDGE_CURVE('',#3145,#3146,#1853,.T.);
#3729=EDGE_CURVE('',#3146,#3146,#2903,.T.);
#3730=EDGE_CURVE('',#3147,#3148,#1854,.T.);
#3731=EDGE_CURVE('',#3149,#3147,#1855,.T.);
#3732=EDGE_CURVE('',#3150,#3149,#1856,.T.);
#3733=EDGE_CURVE('',#3150,#3148,#1857,.T.);
#3734=EDGE_CURVE('',#3149,#3151,#1858,.T.);
#3735=EDGE_CURVE('',#3151,#3152,#1859,.T.);
#3736=EDGE_CURVE('',#3152,#3150,#1860,.T.);
#3737=EDGE_CURVE('',#3153,#3154,#1861,.T.);
#3738=EDGE_CURVE('',#3155,#3154,#1862,.T.);
#3739=EDGE_CURVE('',#3156,#3155,#1863,.T.);
#3740=EDGE_CURVE('',#3156,#3153,#1864,.T.);
#3741=EDGE_CURVE('',#3147,#3157,#1865,.T.);
#3742=EDGE_CURVE('',#3154,#3157,#1866,.T.);
#3743=EDGE_CURVE('',#3153,#3151,#1867,.T.);
#3744=EDGE_CURVE('',#3158,#3155,#1868,.T.);
#3745=EDGE_CURVE('',#3148,#3158,#1869,.T.);
#3746=EDGE_CURVE('',#3152,#3156,#1870,.T.);
#3747=EDGE_CURVE('',#3157,#3158,#1871,.T.);
#3748=EDGE_CURVE('',#3159,#3159,#2904,.T.);
#3749=EDGE_CURVE('',#3159,#3160,#1872,.T.);
#3750=EDGE_CURVE('',#3160,#3160,#2905,.T.);
#3751=EDGE_CURVE('',#3161,#3161,#2906,.T.);
#3752=EDGE_CURVE('',#3161,#3162,#1873,.T.);
#3753=EDGE_CURVE('',#3162,#3162,#2907,.T.);
#3754=EDGE_CURVE('',#3163,#3163,#2908,.T.);
#3755=EDGE_CURVE('',#3163,#3164,#1874,.T.);
#3756=EDGE_CURVE('',#3164,#3164,#2909,.T.);
#3757=EDGE_CURVE('',#3165,#3165,#2910,.T.);
#3758=EDGE_CURVE('',#3165,#3166,#1875,.T.);
#3759=EDGE_CURVE('',#3166,#3166,#2911,.T.);
#3760=EDGE_CURVE('',#3167,#3167,#2912,.T.);
#3761=EDGE_CURVE('',#3167,#3168,#1876,.T.);
#3762=EDGE_CURVE('',#3168,#3168,#2913,.T.);
#3763=EDGE_CURVE('',#3169,#3169,#2914,.T.);
#3764=EDGE_CURVE('',#3169,#3170,#1877,.T.);
#3765=EDGE_CURVE('',#3170,#3170,#2915,.T.);
#3766=EDGE_CURVE('',#3171,#3171,#2916,.T.);
#3767=EDGE_CURVE('',#3171,#3172,#1878,.T.);
#3768=EDGE_CURVE('',#3172,#3172,#2917,.T.);
#3769=EDGE_CURVE('',#3173,#3173,#2918,.T.);
#3770=EDGE_CURVE('',#3173,#3174,#1879,.T.);
#3771=EDGE_CURVE('',#3174,#3174,#2919,.T.);
#3772=EDGE_CURVE('',#3175,#3176,#1880,.T.);
#3773=EDGE_CURVE('',#3175,#3177,#1881,.T.);
#3774=EDGE_CURVE('',#3178,#3177,#1882,.T.);
#3775=EDGE_CURVE('',#3176,#3178,#1883,.T.);
#3776=EDGE_CURVE('',#3179,#3175,#1884,.T.);
#3777=EDGE_CURVE('',#3179,#3180,#1885,.T.);
#3778=EDGE_CURVE('',#3177,#3180,#1886,.T.);
#3779=EDGE_CURVE('',#3181,#3179,#1887,.T.);
#3780=EDGE_CURVE('',#3181,#3182,#1888,.T.);
#3781=EDGE_CURVE('',#3180,#3182,#1889,.T.);
#3782=EDGE_CURVE('',#3183,#3181,#1890,.T.);
#3783=EDGE_CURVE('',#3183,#3184,#1891,.T.);
#3784=EDGE_CURVE('',#3182,#3184,#1892,.T.);
#3785=EDGE_CURVE('',#3185,#3183,#1893,.T.);
#3786=EDGE_CURVE('',#3185,#3186,#1894,.T.);
#3787=EDGE_CURVE('',#3184,#3186,#1895,.T.);
#3788=EDGE_CURVE('',#3187,#3185,#1896,.T.);
#3789=EDGE_CURVE('',#3187,#3188,#1897,.T.);
#3790=EDGE_CURVE('',#3186,#3188,#1898,.T.);
#3791=EDGE_CURVE('',#3189,#3187,#1899,.T.);
#3792=EDGE_CURVE('',#3189,#3190,#1900,.T.);
#3793=EDGE_CURVE('',#3188,#3190,#1901,.T.);
#3794=EDGE_CURVE('',#3191,#3189,#1902,.T.);
#3795=EDGE_CURVE('',#3191,#3192,#1903,.T.);
#3796=EDGE_CURVE('',#3190,#3192,#1904,.T.);
#3797=EDGE_CURVE('',#3193,#3191,#1905,.T.);
#3798=EDGE_CURVE('',#3194,#3193,#1906,.T.);
#3799=EDGE_CURVE('',#3192,#3194,#1907,.T.);
#3800=EDGE_CURVE('',#3195,#3196,#1908,.T.);
#3801=EDGE_CURVE('',#3195,#3197,#1909,.T.);
#3802=EDGE_CURVE('',#3198,#3197,#1910,.T.);
#3803=EDGE_CURVE('',#3196,#3198,#1911,.T.);
#3804=EDGE_CURVE('',#3199,#3195,#1912,.T.);
#3805=EDGE_CURVE('',#3199,#3200,#1913,.T.);
#3806=EDGE_CURVE('',#3197,#3200,#1914,.T.);
#3807=EDGE_CURVE('',#3201,#3199,#1915,.T.);
#3808=EDGE_CURVE('',#3201,#3202,#1916,.T.);
#3809=EDGE_CURVE('',#3200,#3202,#1917,.T.);
#3810=EDGE_CURVE('',#3203,#3201,#1918,.T.);
#3811=EDGE_CURVE('',#3203,#3204,#1919,.T.);
#3812=EDGE_CURVE('',#3202,#3204,#1920,.T.);
#3813=EDGE_CURVE('',#3205,#3203,#1921,.T.);
#3814=EDGE_CURVE('',#3205,#3206,#1922,.T.);
#3815=EDGE_CURVE('',#3204,#3206,#1923,.T.);
#3816=EDGE_CURVE('',#3207,#3205,#1924,.T.);
#3817=EDGE_CURVE('',#3207,#3208,#1925,.T.);
#3818=EDGE_CURVE('',#3206,#3208,#1926,.T.);
#3819=EDGE_CURVE('',#3209,#3207,#1927,.T.);
#3820=EDGE_CURVE('',#3209,#3210,#1928,.T.);
#3821=EDGE_CURVE('',#3208,#3210,#1929,.T.);
#3822=EDGE_CURVE('',#3211,#3209,#1930,.T.);
#3823=EDGE_CURVE('',#3211,#3212,#1931,.T.);
#3824=EDGE_CURVE('',#3210,#3212,#1932,.T.);
#3825=EDGE_CURVE('',#3213,#3211,#1933,.T.);
#3826=EDGE_CURVE('',#3214,#3213,#1934,.T.);
#3827=EDGE_CURVE('',#3212,#3214,#1935,.T.);
#3828=EDGE_CURVE('',#3215,#3216,#1936,.T.);
#3829=EDGE_CURVE('',#3215,#3217,#1937,.T.);
#3830=EDGE_CURVE('',#3218,#3217,#1938,.T.);
#3831=EDGE_CURVE('',#3216,#3218,#1939,.T.);
#3832=EDGE_CURVE('',#3219,#3215,#1940,.T.);
#3833=EDGE_CURVE('',#3219,#3220,#1941,.T.);
#3834=EDGE_CURVE('',#3217,#3220,#1942,.T.);
#3835=EDGE_CURVE('',#3221,#3219,#1943,.T.);
#3836=EDGE_CURVE('',#3221,#3222,#1944,.T.);
#3837=EDGE_CURVE('',#3220,#3222,#1945,.T.);
#3838=EDGE_CURVE('',#3223,#3221,#1946,.T.);
#3839=EDGE_CURVE('',#3223,#3224,#1947,.T.);
#3840=EDGE_CURVE('',#3222,#3224,#1948,.T.);
#3841=EDGE_CURVE('',#3225,#3223,#1949,.T.);
#3842=EDGE_CURVE('',#3225,#3226,#1950,.T.);
#3843=EDGE_CURVE('',#3224,#3226,#1951,.T.);
#3844=EDGE_CURVE('',#3227,#3225,#1952,.T.);
#3845=EDGE_CURVE('',#3227,#3228,#1953,.T.);
#3846=EDGE_CURVE('',#3226,#3228,#1954,.T.);
#3847=EDGE_CURVE('',#3229,#3227,#1955,.T.);
#3848=EDGE_CURVE('',#3229,#3230,#1956,.T.);
#3849=EDGE_CURVE('',#3228,#3230,#1957,.T.);
#3850=EDGE_CURVE('',#3231,#3229,#1958,.T.);
#3851=EDGE_CURVE('',#3231,#3232,#1959,.T.);
#3852=EDGE_CURVE('',#3230,#3232,#1960,.T.);
#3853=EDGE_CURVE('',#3233,#3231,#1961,.T.);
#3854=EDGE_CURVE('',#3234,#3233,#1962,.T.);
#3855=EDGE_CURVE('',#3232,#3234,#1963,.T.);
#3856=EDGE_CURVE('',#3235,#3236,#1964,.T.);
#3857=EDGE_CURVE('',#3235,#3237,#1965,.T.);
#3858=EDGE_CURVE('',#3238,#3237,#1966,.T.);
#3859=EDGE_CURVE('',#3236,#3238,#1967,.T.);
#3860=EDGE_CURVE('',#3239,#3235,#1968,.T.);
#3861=EDGE_CURVE('',#3239,#3240,#1969,.T.);
#3862=EDGE_CURVE('',#3237,#3240,#1970,.T.);
#3863=EDGE_CURVE('',#3241,#3239,#1971,.T.);
#3864=EDGE_CURVE('',#3241,#3242,#1972,.T.);
#3865=EDGE_CURVE('',#3240,#3242,#1973,.T.);
#3866=EDGE_CURVE('',#3243,#3241,#1974,.T.);
#3867=EDGE_CURVE('',#3243,#3244,#1975,.T.);
#3868=EDGE_CURVE('',#3242,#3244,#1976,.T.);
#3869=EDGE_CURVE('',#3245,#3243,#1977,.T.);
#3870=EDGE_CURVE('',#3245,#3246,#1978,.T.);
#3871=EDGE_CURVE('',#3244,#3246,#1979,.T.);
#3872=EDGE_CURVE('',#3247,#3245,#1980,.T.);
#3873=EDGE_CURVE('',#3247,#3248,#1981,.T.);
#3874=EDGE_CURVE('',#3246,#3248,#1982,.T.);
#3875=EDGE_CURVE('',#3249,#3247,#1983,.T.);
#3876=EDGE_CURVE('',#3249,#3250,#1984,.T.);
#3877=EDGE_CURVE('',#3248,#3250,#1985,.T.);
#3878=EDGE_CURVE('',#3251,#3249,#1986,.T.);
#3879=EDGE_CURVE('',#3251,#3252,#1987,.T.);
#3880=EDGE_CURVE('',#3250,#3252,#1988,.T.);
#3881=EDGE_CURVE('',#3253,#3251,#1989,.T.);
#3882=EDGE_CURVE('',#3254,#3253,#1990,.T.);
#3883=EDGE_CURVE('',#3252,#3254,#1991,.T.);
#3884=EDGE_CURVE('',#3255,#3255,#2920,.T.);
#3885=EDGE_CURVE('',#3255,#3256,#1992,.T.);
#3886=EDGE_CURVE('',#3256,#3256,#2921,.T.);
#3887=EDGE_CURVE('',#3193,#3257,#1993,.T.);
#3888=EDGE_CURVE('',#3257,#3258,#1994,.T.);
#3889=EDGE_CURVE('',#3194,#3258,#1995,.T.);
#3890=EDGE_CURVE('',#3259,#3178,#1996,.T.);
#3891=EDGE_CURVE('',#3260,#3259,#1997,.T.);
#3892=EDGE_CURVE('',#3260,#3176,#1998,.T.);
#3893=EDGE_CURVE('',#3213,#3260,#1999,.T.);
#3894=EDGE_CURVE('',#3214,#3259,#2000,.T.);
#3895=EDGE_CURVE('',#3261,#3198,#2001,.T.);
#3896=EDGE_CURVE('',#3262,#3261,#2002,.T.);
#3897=EDGE_CURVE('',#3262,#3196,#2003,.T.);
#3898=EDGE_CURVE('',#3233,#3262,#2004,.T.);
#3899=EDGE_CURVE('',#3234,#3261,#2005,.T.);
#3900=EDGE_CURVE('',#3263,#3218,#2006,.T.);
#3901=EDGE_CURVE('',#3264,#3263,#2007,.T.);
#3902=EDGE_CURVE('',#3264,#3216,#2008,.T.);
#3903=EDGE_CURVE('',#3253,#3264,#2009,.T.);
#3904=EDGE_CURVE('',#3254,#3263,#2010,.T.);
#3905=EDGE_CURVE('',#3258,#3238,#2011,.T.);
#3906=EDGE_CURVE('',#3257,#3236,#2012,.T.);
#3907=EDGE_CURVE('',#3265,#3266,#2013,.T.);
#3908=EDGE_CURVE('',#3267,#3265,#2014,.T.);
#3909=EDGE_CURVE('',#3268,#3267,#2015,.T.);
#3910=EDGE_CURVE('',#3266,#3268,#2016,.T.);
#3911=EDGE_CURVE('',#3267,#3269,#2017,.T.);
#3912=EDGE_CURVE('',#3270,#3269,#2018,.T.);
#3913=EDGE_CURVE('',#3268,#3270,#2019,.T.);
#3914=EDGE_CURVE('',#3269,#3271,#2020,.T.);
#3915=EDGE_CURVE('',#3271,#3272,#2021,.T.);
#3916=EDGE_CURVE('',#3272,#3270,#2022,.T.);
#3917=EDGE_CURVE('',#3273,#3273,#2922,.T.);
#3918=EDGE_CURVE('',#3274,#3265,#2023,.T.);
#3919=EDGE_CURVE('',#3275,#3274,#2024,.T.);
#3920=EDGE_CURVE('',#3275,#3276,#2025,.T.);
#3921=EDGE_CURVE('',#3277,#3276,#2026,.T.);
#3922=EDGE_CURVE('',#3277,#3278,#2027,.T.);
#3923=EDGE_CURVE('',#3278,#3279,#2028,.T.);
#3924=EDGE_CURVE('',#3279,#3271,#2029,.T.);
#3925=EDGE_CURVE('',#3279,#3280,#2030,.T.);
#3926=EDGE_CURVE('',#3280,#3272,#2031,.T.);
#3927=EDGE_CURVE('',#3281,#3278,#2032,.T.);
#3928=EDGE_CURVE('',#3280,#3281,#2033,.T.);
#3929=EDGE_CURVE('',#3282,#3281,#2034,.T.);
#3930=EDGE_CURVE('',#3283,#3282,#2035,.T.);
#3931=EDGE_CURVE('',#3283,#3284,#2036,.T.);
#3932=EDGE_CURVE('',#3285,#3284,#2037,.T.);
#3933=EDGE_CURVE('',#3285,#3266,#2038,.T.);
#3934=EDGE_CURVE('',#3282,#3277,#2039,.T.);
#3935=EDGE_CURVE('',#3276,#3286,#2040,.T.);
#3936=EDGE_CURVE('',#3286,#3287,#413,.T.);
#3937=EDGE_CURVE('',#3287,#3283,#2041,.T.);
#3938=EDGE_CURVE('',#3288,#3286,#2923,.F.);
#3939=EDGE_CURVE('',#3288,#3273,#2042,.T.);
#3940=EDGE_CURVE('',#3289,#3288,#2924,.F.);
#3941=EDGE_CURVE('',#3290,#3289,#414,.T.);
#3942=EDGE_CURVE('',#3287,#3290,#2925,.F.);
#3943=EDGE_CURVE('',#3289,#3275,#2043,.T.);
#3944=EDGE_CURVE('',#3284,#3290,#2044,.T.);
#3945=EDGE_CURVE('',#3274,#3285,#2045,.T.);
#3946=EDGE_CURVE('',#3291,#3292,#2046,.T.);
#3947=EDGE_CURVE('',#3292,#3293,#2047,.T.);
#3948=EDGE_CURVE('',#3293,#3294,#2048,.T.);
#3949=EDGE_CURVE('',#3291,#3294,#2049,.T.);
#3950=EDGE_CURVE('',#3292,#3295,#2050,.T.);
#3951=EDGE_CURVE('',#3295,#3296,#2051,.T.);
#3952=EDGE_CURVE('',#3296,#3293,#2052,.T.);
#3953=EDGE_CURVE('',#3295,#3297,#2053,.T.);
#3954=EDGE_CURVE('',#3297,#3298,#2054,.T.);
#3955=EDGE_CURVE('',#3298,#3296,#2055,.T.);
#3956=EDGE_CURVE('',#3297,#3299,#2056,.T.);
#3957=EDGE_CURVE('',#3299,#3300,#2057,.T.);
#3958=EDGE_CURVE('',#3300,#3298,#2058,.T.);
#3959=EDGE_CURVE('',#3299,#3301,#2059,.T.);
#3960=EDGE_CURVE('',#3301,#3302,#2060,.T.);
#3961=EDGE_CURVE('',#3302,#3300,#2061,.T.);
#3962=EDGE_CURVE('',#3301,#3291,#2062,.T.);
#3963=EDGE_CURVE('',#3294,#3302,#2063,.T.);
#3964=EDGE_CURVE('',#3303,#3303,#2926,.T.);
#3965=EDGE_CURVE('',#3304,#3304,#2927,.T.);
#3966=EDGE_CURVE('',#3305,#3305,#2928,.T.);
#3967=EDGE_CURVE('',#3305,#3304,#2064,.T.);
#3968=EDGE_CURVE('',#3306,#3306,#2929,.T.);
#3969=EDGE_CURVE('',#3306,#3305,#2065,.T.);
#3970=EDGE_CURVE('',#3307,#3307,#2930,.T.);
#3971=EDGE_CURVE('',#3307,#3306,#2066,.T.);
#3972=EDGE_CURVE('',#3308,#3308,#2931,.T.);
#3973=EDGE_CURVE('',#3309,#3309,#2932,.F.);
#3974=EDGE_CURVE('',#3309,#3308,#2067,.T.);
#3975=EDGE_CURVE('',#3303,#3309,#2068,.T.);
#3976=EDGE_CURVE('',#3310,#3311,#2069,.T.);
#3977=EDGE_CURVE('',#3311,#3312,#2070,.T.);
#3978=EDGE_CURVE('',#3312,#3313,#2071,.T.);
#3979=EDGE_CURVE('',#3310,#3313,#2072,.T.);
#3980=EDGE_CURVE('',#3311,#3314,#2073,.T.);
#3981=EDGE_CURVE('',#3314,#3315,#2074,.T.);
#3982=EDGE_CURVE('',#3315,#3312,#2075,.T.);
#3983=EDGE_CURVE('',#3314,#3316,#2076,.T.);
#3984=EDGE_CURVE('',#3316,#3317,#2077,.T.);
#3985=EDGE_CURVE('',#3317,#3315,#2078,.T.);
#3986=EDGE_CURVE('',#3316,#3318,#2079,.T.);
#3987=EDGE_CURVE('',#3318,#3319,#2080,.T.);
#3988=EDGE_CURVE('',#3319,#3317,#2081,.T.);
#3989=EDGE_CURVE('',#3318,#3320,#2082,.T.);
#3990=EDGE_CURVE('',#3320,#3321,#2083,.T.);
#3991=EDGE_CURVE('',#3321,#3319,#2084,.T.);
#3992=EDGE_CURVE('',#3320,#3310,#2085,.T.);
#3993=EDGE_CURVE('',#3313,#3321,#2086,.T.);
#3994=EDGE_CURVE('',#3322,#3322,#2933,.T.);
#3995=EDGE_CURVE('',#3323,#3323,#2934,.T.);
#3996=EDGE_CURVE('',#3324,#3324,#2935,.T.);
#3997=EDGE_CURVE('',#3324,#3323,#2087,.T.);
#3998=EDGE_CURVE('',#3325,#3325,#2936,.T.);
#3999=EDGE_CURVE('',#3325,#3324,#2088,.T.);
#4000=EDGE_CURVE('',#3326,#3326,#2937,.T.);
#4001=EDGE_CURVE('',#3326,#3325,#2089,.T.);
#4002=EDGE_CURVE('',#3327,#3327,#2938,.T.);
#4003=EDGE_CURVE('',#3328,#3328,#2939,.F.);
#4004=EDGE_CURVE('',#3328,#3327,#2090,.T.);
#4005=EDGE_CURVE('',#3322,#3328,#2091,.T.);
#4006=EDGE_CURVE('',#3329,#3329,#2940,.T.);
#4007=EDGE_CURVE('',#3329,#3330,#2092,.T.);
#4008=EDGE_CURVE('',#3330,#3330,#2941,.T.);
#4009=EDGE_CURVE('',#3331,#3331,#2942,.T.);
#4010=EDGE_CURVE('',#3331,#3332,#2093,.T.);
#4011=EDGE_CURVE('',#3332,#3332,#2943,.T.);
#4012=EDGE_CURVE('',#3333,#3334,#2944,.T.);
#4013=EDGE_CURVE('',#3335,#3335,#2945,.T.);
#4014=EDGE_CURVE('',#3335,#3336,#2094,.T.);
#4015=EDGE_CURVE('',#3336,#3336,#2946,.T.);
#4016=EDGE_CURVE('',#3337,#3337,#2947,.T.);
#4017=EDGE_CURVE('',#3337,#3338,#2095,.T.);
#4018=EDGE_CURVE('',#3338,#3338,#2948,.T.);
#4019=EDGE_CURVE('',#3339,#3339,#2949,.T.);
#4020=EDGE_CURVE('',#3339,#3340,#2096,.T.);
#4021=EDGE_CURVE('',#3340,#3340,#2950,.T.);
#4022=EDGE_CURVE('',#3341,#3341,#2951,.T.);
#4023=EDGE_CURVE('',#3341,#3342,#2097,.T.);
#4024=EDGE_CURVE('',#3342,#3342,#2952,.T.);
#4025=EDGE_CURVE('',#3343,#3343,#2953,.T.);
#4026=EDGE_CURVE('',#3343,#3344,#2098,.T.);
#4027=EDGE_CURVE('',#3344,#3344,#2954,.T.);
#4028=EDGE_CURVE('',#3345,#3345,#2955,.T.);
#4029=EDGE_CURVE('',#3345,#3346,#2099,.T.);
#4030=EDGE_CURVE('',#3346,#3346,#2956,.T.);
#4031=EDGE_CURVE('',#3347,#3348,#2100,.T.);
#4032=EDGE_CURVE('',#3348,#3349,#2101,.T.);
#4033=EDGE_CURVE('',#3350,#3349,#2102,.T.);
#4034=EDGE_CURVE('',#3347,#3350,#2103,.T.);
#4035=EDGE_CURVE('',#3351,#3347,#2104,.T.);
#4036=EDGE_CURVE('',#3352,#3350,#2105,.T.);
#4037=EDGE_CURVE('',#3351,#3352,#2106,.T.);
#4038=EDGE_CURVE('',#3353,#3351,#2107,.T.);
#4039=EDGE_CURVE('',#3354,#3352,#2108,.T.);
#4040=EDGE_CURVE('',#3353,#3354,#2109,.T.);
#4041=EDGE_CURVE('',#3355,#3353,#2110,.T.);
#4042=EDGE_CURVE('',#3356,#3354,#2111,.T.);
#4043=EDGE_CURVE('',#3355,#3356,#2112,.T.);
#4044=EDGE_CURVE('',#3357,#3355,#2113,.T.);
#4045=EDGE_CURVE('',#3358,#3356,#2114,.T.);
#4046=EDGE_CURVE('',#3357,#3358,#2115,.T.);
#4047=EDGE_CURVE('',#3359,#3357,#2116,.T.);
#4048=EDGE_CURVE('',#3360,#3358,#2117,.T.);
#4049=EDGE_CURVE('',#3359,#3360,#2118,.T.);
#4050=EDGE_CURVE('',#3361,#3359,#2119,.T.);
#4051=EDGE_CURVE('',#3362,#3360,#2120,.T.);
#4052=EDGE_CURVE('',#3361,#3362,#2121,.T.);
#4053=EDGE_CURVE('',#3348,#3361,#2122,.T.);
#4054=EDGE_CURVE('',#3349,#3362,#2123,.T.);
#4055=EDGE_CURVE('',#3363,#3363,#2957,.T.);
#4056=EDGE_CURVE('',#3363,#3364,#2124,.T.);
#4057=EDGE_CURVE('',#3364,#3364,#2958,.T.);
#4058=EDGE_CURVE('',#3365,#3365,#2959,.T.);
#4059=EDGE_CURVE('',#3366,#3367,#2960,.T.);
#4060=EDGE_CURVE('',#3368,#3368,#2961,.T.);
#4061=EDGE_CURVE('',#3369,#3370,#363,.T.);
#4062=EDGE_CURVE('',#3371,#3369,#364,.T.);
#4063=EDGE_CURVE('',#3370,#3371,#365,.T.);
#4064=EDGE_CURVE('',#3370,#3372,#2125,.T.);
#4065=EDGE_CURVE('',#3372,#3372,#366,.T.);
#4066=EDGE_CURVE('',#3373,#3373,#367,.T.);
#4067=EDGE_CURVE('',#3373,#3374,#2126,.T.);
#4068=EDGE_CURVE('',#3375,#3374,#368,.T.);
#4069=EDGE_CURVE('',#3376,#3375,#369,.T.);
#4070=EDGE_CURVE('',#3374,#3376,#370,.T.);
#4071=EDGE_CURVE('',#3377,#3377,#2962,.T.);
#4072=EDGE_CURVE('',#3377,#3378,#2127,.T.);
#4073=EDGE_CURVE('',#3378,#3378,#2963,.T.);
#4074=EDGE_CURVE('',#3379,#3380,#371,.T.);
#4075=EDGE_CURVE('',#3380,#3381,#372,.T.);
#4076=EDGE_CURVE('',#3381,#3379,#373,.T.);
#4077=EDGE_CURVE('',#3382,#3383,#374,.T.);
#4078=EDGE_CURVE('',#3383,#3384,#375,.T.);
#4079=EDGE_CURVE('',#3384,#3382,#376,.T.);
#4080=EDGE_CURVE('',#3385,#3386,#377,.T.);
#4081=EDGE_CURVE('',#3386,#3387,#378,.T.);
#4082=EDGE_CURVE('',#3387,#3385,#379,.T.);
#4083=EDGE_CURVE('',#3388,#3389,#380,.T.);
#4084=EDGE_CURVE('',#3389,#3390,#381,.T.);
#4085=EDGE_CURVE('',#3390,#3388,#382,.T.);
#4086=EDGE_CURVE('',#3381,#3391,#2128,.T.);
#4087=EDGE_CURVE('',#3391,#3391,#383,.T.);
#4088=EDGE_CURVE('',#3392,#3392,#384,.T.);
#4089=EDGE_CURVE('',#3392,#3384,#2129,.T.);
#4090=EDGE_CURVE('',#3387,#3393,#2130,.T.);
#4091=EDGE_CURVE('',#3393,#3393,#385,.T.);
#4092=EDGE_CURVE('',#3394,#3394,#386,.T.);
#4093=EDGE_CURVE('',#3394,#3390,#2131,.T.);
#4094=EDGE_CURVE('',#3395,#3395,#2964,.T.);
#4095=EDGE_CURVE('',#3396,#3396,#2965,.T.);
#4096=EDGE_CURVE('',#3397,#3397,#2966,.T.);
#4097=EDGE_CURVE('',#3397,#3396,#2132,.T.);
#4098=EDGE_CURVE('',#3398,#3398,#2967,.T.);
#4099=EDGE_CURVE('',#3398,#3395,#2133,.T.);
#4100=EDGE_CURVE('',#3399,#3399,#2968,.T.);
#4101=EDGE_CURVE('',#3400,#3400,#2969,.T.);
#4102=EDGE_CURVE('',#3400,#3399,#2134,.T.);
#4103=EDGE_CURVE('',#3401,#3401,#2970,.T.);
#4104=EDGE_CURVE('',#3401,#3400,#2135,.T.);
#4105=EDGE_CURVE('',#3402,#3402,#2971,.T.);
#4106=EDGE_CURVE('',#3402,#3401,#2136,.T.);
#4107=EDGE_CURVE('',#3403,#3403,#2972,.T.);
#4108=EDGE_CURVE('',#3404,#3404,#2973,.F.);
#4109=EDGE_CURVE('',#3404,#3403,#2137,.T.);
#4110=EDGE_CURVE('',#3405,#3405,#2974,.F.);
#4111=EDGE_CURVE('',#3405,#3404,#2138,.T.);
#4112=EDGE_CURVE('',#3406,#3406,#2975,.T.);
#4113=EDGE_CURVE('',#3406,#3405,#2139,.T.);
#4114=EDGE_CURVE('',#3407,#3408,#2140,.T.);
#4115=EDGE_CURVE('',#3408,#3409,#2141,.T.);
#4116=EDGE_CURVE('',#3409,#3410,#2142,.T.);
#4117=EDGE_CURVE('',#3407,#3410,#2143,.T.);
#4118=EDGE_CURVE('',#3408,#3411,#2144,.T.);
#4119=EDGE_CURVE('',#3411,#3412,#2145,.T.);
#4120=EDGE_CURVE('',#3412,#3409,#2146,.T.);
#4121=EDGE_CURVE('',#3411,#3413,#2147,.T.);
#4122=EDGE_CURVE('',#3413,#3414,#2148,.T.);
#4123=EDGE_CURVE('',#3414,#3412,#2149,.T.);
#4124=EDGE_CURVE('',#3413,#3415,#2150,.T.);
#4125=EDGE_CURVE('',#3415,#3416,#2151,.T.);
#4126=EDGE_CURVE('',#3416,#3414,#2152,.T.);
#4127=EDGE_CURVE('',#3415,#3417,#2153,.T.);
#4128=EDGE_CURVE('',#3417,#3418,#2154,.T.);
#4129=EDGE_CURVE('',#3418,#3416,#2155,.T.);
#4130=EDGE_CURVE('',#3417,#3407,#2156,.T.);
#4131=EDGE_CURVE('',#3410,#3418,#2157,.T.);
#4132=EDGE_CURVE('',#3419,#3419,#2976,.T.);
#4133=EDGE_CURVE('',#3419,#3420,#2158,.T.);
#4134=EDGE_CURVE('',#3420,#3420,#2977,.T.);
#4135=EDGE_CURVE('',#3421,#3421,#2978,.T.);
#4136=EDGE_CURVE('',#3421,#3422,#2159,.T.);
#4137=EDGE_CURVE('',#3422,#3422,#2979,.T.);
#4138=EDGE_CURVE('',#3423,#3424,#11,.T.);
#4139=EDGE_CURVE('',#3425,#3423,#12,.T.);
#4140=EDGE_CURVE('',#3425,#3426,#2160,.T.);
#4141=EDGE_CURVE('',#3426,#3426,#2980,.T.);
#4142=EDGE_CURVE('',#3427,#3425,#13,.T.);
#4143=EDGE_CURVE('',#3428,#3427,#14,.T.);
#4144=EDGE_CURVE('',#3429,#3428,#15,.T.);
#4145=EDGE_CURVE('',#3424,#3429,#16,.T.);
#4146=EDGE_CURVE('',#3430,#3430,#2981,.T.);
#4147=EDGE_CURVE('',#3430,#3431,#2161,.T.);
#4148=EDGE_CURVE('',#3432,#3431,#17,.T.);
#4149=EDGE_CURVE('',#3433,#3432,#18,.T.);
#4150=EDGE_CURVE('',#3434,#3433,#19,.T.);
#4151=EDGE_CURVE('',#3435,#3434,#20,.T.);
#4152=EDGE_CURVE('',#3436,#3435,#21,.T.);
#4153=EDGE_CURVE('',#3431,#3436,#22,.T.);
#4154=EDGE_CURVE('',#3427,#3436,#2162,.T.);
#4155=EDGE_CURVE('',#3428,#3435,#2163,.T.);
#4156=EDGE_CURVE('',#3425,#3431,#2164,.T.);
#4157=EDGE_CURVE('',#3423,#3432,#2165,.T.);
#4158=EDGE_CURVE('',#3437,#3437,#2982,.F.);
#4159=EDGE_CURVE('',#3437,#3438,#2166,.T.);
#4160=EDGE_CURVE('',#3438,#3438,#2983,.F.);
#4161=EDGE_CURVE('',#3424,#3433,#2167,.T.);
#4162=EDGE_CURVE('',#3429,#3434,#2168,.T.);
#4163=EDGE_CURVE('',#3439,#3440,#2169,.T.);
#4164=EDGE_CURVE('',#3439,#3441,#2170,.T.);
#4165=EDGE_CURVE('',#3442,#3441,#2171,.T.);
#4166=EDGE_CURVE('',#3442,#3440,#2172,.T.);
#4167=EDGE_CURVE('',#3440,#3443,#2984,.T.);
#4168=EDGE_CURVE('',#3444,#3442,#2173,.T.);
#4169=EDGE_CURVE('',#3443,#3444,#2174,.T.);
#4170=EDGE_CURVE('',#3443,#3445,#2175,.T.);
#4171=EDGE_CURVE('',#3444,#3446,#2176,.T.);
#4172=EDGE_CURVE('',#3446,#3445,#2177,.T.);
#4173=EDGE_CURVE('',#3441,#3446,#2178,.T.);
#4174=EDGE_CURVE('',#3445,#3439,#2985,.T.);
#4175=EDGE_CURVE('',#3447,#3447,#2986,.T.);
#4176=EDGE_CURVE('',#3448,#3448,#2987,.T.);
#4177=EDGE_CURVE('',#3449,#3449,#2988,.T.);
#4178=EDGE_CURVE('',#3450,#3450,#2989,.T.);
#4179=EDGE_CURVE('',#3447,#3449,#2179,.T.);
#4180=EDGE_CURVE('',#3450,#3451,#2180,.T.);
#4181=EDGE_CURVE('',#3451,#3451,#2990,.T.);
#4182=EDGE_CURVE('',#3452,#3452,#2991,.T.);
#4183=EDGE_CURVE('',#3452,#3448,#2181,.T.);
#4184=EDGE_CURVE('',#3453,#3453,#2992,.T.);
#4185=EDGE_CURVE('',#3453,#3454,#2182,.T.);
#4186=EDGE_CURVE('',#3454,#3454,#2993,.T.);
#4187=EDGE_CURVE('',#3455,#3455,#2994,.T.);
#4188=EDGE_CURVE('',#3455,#3456,#2183,.T.);
#4189=EDGE_CURVE('',#3456,#3456,#2995,.T.);
#4190=EDGE_CURVE('',#3457,#3457,#2996,.T.);
#4191=EDGE_CURVE('',#3457,#3458,#2184,.T.);
#4192=EDGE_CURVE('',#3458,#3458,#2997,.T.);
#4193=EDGE_CURVE('',#3459,#3459,#2998,.T.);
#4194=EDGE_CURVE('',#3459,#3460,#2185,.T.);
#4195=EDGE_CURVE('',#3460,#3460,#2999,.T.);
#4196=EDGE_CURVE('',#3461,#3461,#3000,.T.);
#4197=EDGE_CURVE('',#3461,#3462,#2186,.T.);
#4198=EDGE_CURVE('',#3462,#3462,#3001,.T.);
#4199=EDGE_CURVE('',#3463,#3464,#2187,.T.);
#4200=EDGE_CURVE('',#3463,#3465,#2188,.T.);
#4201=EDGE_CURVE('',#3466,#3465,#2189,.T.);
#4202=EDGE_CURVE('',#3464,#3466,#2190,.T.);
#4203=EDGE_CURVE('',#3464,#3467,#2191,.T.);
#4204=EDGE_CURVE('',#3468,#3466,#2192,.T.);
#4205=EDGE_CURVE('',#3467,#3468,#2193,.T.);
#4206=EDGE_CURVE('',#3467,#3469,#2194,.T.);
#4207=EDGE_CURVE('',#3470,#3468,#2195,.T.);
#4208=EDGE_CURVE('',#3469,#3470,#2196,.T.);
#4209=EDGE_CURVE('',#3469,#3471,#2197,.T.);
#4210=EDGE_CURVE('',#3472,#3470,#2198,.T.);
#4211=EDGE_CURVE('',#3471,#3472,#2199,.T.);
#4212=EDGE_CURVE('',#3471,#3473,#2200,.T.);
#4213=EDGE_CURVE('',#3474,#3472,#2201,.T.);
#4214=EDGE_CURVE('',#3473,#3474,#2202,.T.);
#4215=EDGE_CURVE('',#3473,#3463,#2203,.T.);
#4216=EDGE_CURVE('',#3465,#3474,#2204,.T.);
#4217=EDGE_CURVE('',#3475,#3475,#3002,.T.);
#4218=EDGE_CURVE('',#3475,#3476,#2205,.T.);
#4219=EDGE_CURVE('',#3476,#3476,#3003,.T.);
#4220=EDGE_CURVE('',#3477,#3478,#2206,.T.);
#4221=EDGE_CURVE('',#3477,#3479,#2207,.T.);
#4222=EDGE_CURVE('',#3480,#3479,#2208,.T.);
#4223=EDGE_CURVE('',#3478,#3480,#2209,.T.);
#4224=EDGE_CURVE('',#3478,#3481,#2210,.T.);
#4225=EDGE_CURVE('',#3482,#3480,#2211,.T.);
#4226=EDGE_CURVE('',#3481,#3482,#2212,.T.);
#4227=EDGE_CURVE('',#3481,#3483,#2213,.T.);
#4228=EDGE_CURVE('',#3484,#3482,#2214,.T.);
#4229=EDGE_CURVE('',#3483,#3484,#2215,.T.);
#4230=EDGE_CURVE('',#3483,#3485,#2216,.T.);
#4231=EDGE_CURVE('',#3486,#3484,#2217,.T.);
#4232=EDGE_CURVE('',#3485,#3486,#2218,.T.);
#4233=EDGE_CURVE('',#3485,#3487,#2219,.T.);
#4234=EDGE_CURVE('',#3488,#3486,#2220,.T.);
#4235=EDGE_CURVE('',#3487,#3488,#2221,.T.);
#4236=EDGE_CURVE('',#3487,#3477,#2222,.T.);
#4237=EDGE_CURVE('',#3479,#3488,#2223,.T.);
#4238=EDGE_CURVE('',#3489,#3490,#2224,.T.);
#4239=EDGE_CURVE('',#3489,#3490,#3004,.T.);
#4240=EDGE_CURVE('',#3491,#3489,#387,.T.);
#4241=EDGE_CURVE('',#3492,#3491,#3005,.T.);
#4242=EDGE_CURVE('',#3492,#3493,#2225,.T.);
#4243=EDGE_CURVE('',#3494,#3493,#388,.T.);
#4244=EDGE_CURVE('',#3493,#3494,#389,.T.);
#4245=EDGE_CURVE('',#3495,#3492,#3006,.T.);
#4246=EDGE_CURVE('',#3490,#3495,#390,.T.);
#4247=EDGE_CURVE('',#3495,#3491,#2226,.T.);
#4248=EDGE_CURVE('',#3496,#3497,#2227,.T.);
#4249=EDGE_CURVE('',#3496,#3498,#2228,.T.);
#4250=EDGE_CURVE('',#3499,#3498,#2229,.T.);
#4251=EDGE_CURVE('',#3497,#3499,#2230,.T.);
#4252=EDGE_CURVE('',#3500,#3496,#2231,.T.);
#4253=EDGE_CURVE('',#3500,#3501,#2232,.T.);
#4254=EDGE_CURVE('',#3498,#3501,#2233,.T.);
#4255=EDGE_CURVE('',#3502,#3500,#2234,.T.);
#4256=EDGE_CURVE('',#3503,#3502,#2235,.T.);
#4257=EDGE_CURVE('',#3501,#3503,#2236,.T.);
#4258=EDGE_CURVE('',#3504,#3504,#3007,.T.);
#4259=EDGE_CURVE('',#3503,#3499,#3008,.T.);
#4260=EDGE_CURVE('',#3502,#3497,#3009,.T.);
#4261=EDGE_CURVE('',#3505,#3505,#3010,.T.);
#4262=EDGE_CURVE('',#3505,#3506,#2237,.T.);
#4263=EDGE_CURVE('',#3506,#3506,#3011,.T.);
#4264=EDGE_CURVE('',#3507,#3507,#3012,.T.);
#4265=EDGE_CURVE('',#3507,#3508,#2238,.T.);
#4266=EDGE_CURVE('',#3508,#3508,#3013,.T.);
#4267=EDGE_CURVE('',#3509,#3509,#3014,.T.);
#4268=EDGE_CURVE('',#3509,#3510,#2239,.T.);
#4269=EDGE_CURVE('',#3510,#3510,#3015,.T.);
#4270=EDGE_CURVE('',#3511,#3511,#3016,.T.);
#4271=EDGE_CURVE('',#3511,#3512,#2240,.T.);
#4272=EDGE_CURVE('',#3512,#3512,#3017,.T.);
#4273=EDGE_CURVE('',#3513,#3513,#3018,.T.);
#4274=EDGE_CURVE('',#3514,#3514,#3019,.T.);
#4275=EDGE_CURVE('',#3515,#3515,#3020,.T.);
#4276=EDGE_CURVE('',#3516,#3516,#3021,.T.);
#4277=EDGE_CURVE('',#3513,#3515,#2241,.T.);
#4278=EDGE_CURVE('',#3516,#3517,#2242,.T.);
#4279=EDGE_CURVE('',#3517,#3517,#3022,.T.);
#4280=EDGE_CURVE('',#3504,#3514,#2243,.T.);
#4281=EDGE_CURVE('',#3518,#3519,#2244,.T.);
#4282=EDGE_CURVE('',#3520,#3518,#2245,.T.);
#4283=EDGE_CURVE('',#3521,#3520,#2246,.T.);
#4284=EDGE_CURVE('',#3522,#3521,#2247,.T.);
#4285=EDGE_CURVE('',#3523,#3522,#2248,.T.);
#4286=EDGE_CURVE('',#3524,#3523,#2249,.T.);
#4287=EDGE_CURVE('',#3525,#3524,#2250,.T.);
#4288=EDGE_CURVE('',#3519,#3525,#2251,.T.);
#4289=EDGE_CURVE('',#3522,#3526,#2252,.T.);
#4290=EDGE_CURVE('',#3526,#3527,#2253,.T.);
#4291=EDGE_CURVE('',#3527,#3523,#2254,.T.);
#4292=EDGE_CURVE('',#3528,#3521,#2255,.T.);
#4293=EDGE_CURVE('',#3528,#3526,#2256,.T.);
#4294=EDGE_CURVE('',#3520,#3529,#2257,.T.);
#4295=EDGE_CURVE('',#3529,#3528,#2258,.T.);
#4296=EDGE_CURVE('',#3530,#3518,#2259,.T.);
#4297=EDGE_CURVE('',#3530,#3529,#2260,.T.);
#4298=EDGE_CURVE('',#3531,#3530,#2261,.T.);
#4299=EDGE_CURVE('',#3532,#3531,#2262,.T.);
#4300=EDGE_CURVE('',#3533,#3532,#2263,.T.);
#4301=EDGE_CURVE('',#3527,#3533,#2264,.T.);
#4302=EDGE_CURVE('',#3519,#3531,#2265,.T.);
#4303=EDGE_CURVE('',#3532,#3525,#2266,.T.);
#4304=EDGE_CURVE('',#3524,#3533,#2267,.T.);
#4305=EDGE_CURVE('',#3534,#3535,#2268,.T.);
#4306=EDGE_CURVE('',#3534,#3536,#2269,.T.);
#4307=EDGE_CURVE('',#3536,#3537,#2270,.T.);
#4308=EDGE_CURVE('',#3535,#3537,#2271,.T.);
#4309=EDGE_CURVE('',#3538,#3534,#2272,.T.);
#4310=EDGE_CURVE('',#3538,#3539,#2273,.T.);
#4311=EDGE_CURVE('',#3539,#3536,#2274,.T.);
#4312=EDGE_CURVE('',#3540,#3538,#2275,.T.);
#4313=EDGE_CURVE('',#3540,#3541,#2276,.T.);
#4314=EDGE_CURVE('',#3541,#3539,#2277,.T.);
#4315=EDGE_CURVE('',#3542,#3540,#2278,.T.);
#4316=EDGE_CURVE('',#3542,#3543,#2279,.T.);
#4317=EDGE_CURVE('',#3543,#3541,#2280,.T.);
#4318=EDGE_CURVE('',#3544,#3542,#2281,.T.);
#4319=EDGE_CURVE('',#3544,#3545,#2282,.T.);
#4320=EDGE_CURVE('',#3545,#3543,#2283,.T.);
#4321=EDGE_CURVE('',#3535,#3544,#2284,.T.);
#4322=EDGE_CURVE('',#3537,#3545,#2285,.T.);
#4323=EDGE_CURVE('',#3546,#3546,#3023,.T.);
#4324=EDGE_CURVE('',#3547,#3547,#3024,.T.);
#4325=EDGE_CURVE('',#3547,#3546,#2286,.T.);
#4326=EDGE_CURVE('',#3548,#3548,#3025,.F.);
#4327=EDGE_CURVE('',#3548,#3547,#2287,.T.);
#4328=EDGE_CURVE('',#3549,#3549,#3026,.T.);
#4329=EDGE_CURVE('',#3549,#3548,#2288,.T.);
#4330=ORIENTED_EDGE('',*,*,#3550,.F.);
#4331=ORIENTED_EDGE('',*,*,#3551,.T.);
#4332=ORIENTED_EDGE('',*,*,#3552,.F.);
#4333=ORIENTED_EDGE('',*,*,#3551,.F.);
#4334=ORIENTED_EDGE('',*,*,#3553,.F.);
#4335=ORIENTED_EDGE('',*,*,#3554,.T.);
#4336=ORIENTED_EDGE('',*,*,#3555,.F.);
#4337=ORIENTED_EDGE('',*,*,#3554,.F.);
#4338=ORIENTED_EDGE('',*,*,#3556,.F.);
#4339=ORIENTED_EDGE('',*,*,#3557,.T.);
#4340=ORIENTED_EDGE('',*,*,#3558,.F.);
#4341=ORIENTED_EDGE('',*,*,#3557,.F.);
#4342=ORIENTED_EDGE('',*,*,#3559,.F.);
#4343=ORIENTED_EDGE('',*,*,#3560,.T.);
#4344=ORIENTED_EDGE('',*,*,#3561,.F.);
#4345=ORIENTED_EDGE('',*,*,#3560,.F.);
#4346=ORIENTED_EDGE('',*,*,#3562,.F.);
#4347=ORIENTED_EDGE('',*,*,#3563,.T.);
#4348=ORIENTED_EDGE('',*,*,#3564,.F.);
#4349=ORIENTED_EDGE('',*,*,#3563,.F.);
#4350=ORIENTED_EDGE('',*,*,#3565,.F.);
#4351=ORIENTED_EDGE('',*,*,#3566,.T.);
#4352=ORIENTED_EDGE('',*,*,#3567,.F.);
#4353=ORIENTED_EDGE('',*,*,#3566,.F.);
#4354=ORIENTED_EDGE('',*,*,#3568,.F.);
#4355=ORIENTED_EDGE('',*,*,#3569,.T.);
#4356=ORIENTED_EDGE('',*,*,#3570,.F.);
#4357=ORIENTED_EDGE('',*,*,#3569,.F.);
#4358=ORIENTED_EDGE('',*,*,#3571,.F.);
#4359=ORIENTED_EDGE('',*,*,#3572,.T.);
#4360=ORIENTED_EDGE('',*,*,#3573,.F.);
#4361=ORIENTED_EDGE('',*,*,#3572,.F.);
#4362=ORIENTED_EDGE('',*,*,#3574,.F.);
#4363=ORIENTED_EDGE('',*,*,#3575,.T.);
#4364=ORIENTED_EDGE('',*,*,#3576,.F.);
#4365=ORIENTED_EDGE('',*,*,#3575,.F.);
#4366=ORIENTED_EDGE('',*,*,#3577,.F.);
#4367=ORIENTED_EDGE('',*,*,#3578,.T.);
#4368=ORIENTED_EDGE('',*,*,#3579,.F.);
#4369=ORIENTED_EDGE('',*,*,#3578,.F.);
#4370=ORIENTED_EDGE('',*,*,#3580,.F.);
#4371=ORIENTED_EDGE('',*,*,#3581,.T.);
#4372=ORIENTED_EDGE('',*,*,#3582,.F.);
#4373=ORIENTED_EDGE('',*,*,#3581,.F.);
#4374=ORIENTED_EDGE('',*,*,#3583,.F.);
#4375=ORIENTED_EDGE('',*,*,#3584,.T.);
#4376=ORIENTED_EDGE('',*,*,#3585,.F.);
#4377=ORIENTED_EDGE('',*,*,#3584,.F.);
#4378=ORIENTED_EDGE('',*,*,#3586,.T.);
#4379=ORIENTED_EDGE('',*,*,#3587,.T.);
#4380=ORIENTED_EDGE('',*,*,#3588,.F.);
#4381=ORIENTED_EDGE('',*,*,#3589,.F.);
#4382=ORIENTED_EDGE('',*,*,#3590,.T.);
#4383=ORIENTED_EDGE('',*,*,#3589,.T.);
#4384=ORIENTED_EDGE('',*,*,#3591,.F.);
#4385=ORIENTED_EDGE('',*,*,#3592,.F.);
#4386=ORIENTED_EDGE('',*,*,#3593,.T.);
#4387=ORIENTED_EDGE('',*,*,#3592,.T.);
#4388=ORIENTED_EDGE('',*,*,#3594,.F.);
#4389=ORIENTED_EDGE('',*,*,#3595,.F.);
#4390=ORIENTED_EDGE('',*,*,#3596,.T.);
#4391=ORIENTED_EDGE('',*,*,#3595,.T.);
#4392=ORIENTED_EDGE('',*,*,#3597,.F.);
#4393=ORIENTED_EDGE('',*,*,#3587,.F.);
#4394=ORIENTED_EDGE('',*,*,#3597,.T.);
#4395=ORIENTED_EDGE('',*,*,#3594,.T.);
#4396=ORIENTED_EDGE('',*,*,#3591,.T.);
#4397=ORIENTED_EDGE('',*,*,#3588,.T.);
#4398=ORIENTED_EDGE('',*,*,#3558,.T.);
#4399=ORIENTED_EDGE('',*,*,#3561,.T.);
#4400=ORIENTED_EDGE('',*,*,#3585,.T.);
#4401=ORIENTED_EDGE('',*,*,#3582,.T.);
#4402=ORIENTED_EDGE('',*,*,#3579,.T.);
#4403=ORIENTED_EDGE('',*,*,#3576,.T.);
#4404=ORIENTED_EDGE('',*,*,#3573,.T.);
#4405=ORIENTED_EDGE('',*,*,#3570,.T.);
#4406=ORIENTED_EDGE('',*,*,#3567,.T.);
#4407=ORIENTED_EDGE('',*,*,#3564,.T.);
#4408=ORIENTED_EDGE('',*,*,#3555,.T.);
#4409=ORIENTED_EDGE('',*,*,#3552,.T.);
#4410=ORIENTED_EDGE('',*,*,#3596,.F.);
#4411=ORIENTED_EDGE('',*,*,#3586,.F.);
#4412=ORIENTED_EDGE('',*,*,#3590,.F.);
#4413=ORIENTED_EDGE('',*,*,#3593,.F.);
#4414=ORIENTED_EDGE('',*,*,#3556,.T.);
#4415=ORIENTED_EDGE('',*,*,#3559,.T.);
#4416=ORIENTED_EDGE('',*,*,#3583,.T.);
#4417=ORIENTED_EDGE('',*,*,#3580,.T.);
#4418=ORIENTED_EDGE('',*,*,#3577,.T.);
#4419=ORIENTED_EDGE('',*,*,#3574,.T.);
#4420=ORIENTED_EDGE('',*,*,#3571,.T.);
#4421=ORIENTED_EDGE('',*,*,#3568,.T.);
#4422=ORIENTED_EDGE('',*,*,#3565,.T.);
#4423=ORIENTED_EDGE('',*,*,#3562,.T.);
#4424=ORIENTED_EDGE('',*,*,#3553,.T.);
#4425=ORIENTED_EDGE('',*,*,#3550,.T.);
#4426=ORIENTED_EDGE('',*,*,#3598,.T.);
#4427=ORIENTED_EDGE('',*,*,#3599,.T.);
#4428=ORIENTED_EDGE('',*,*,#3600,.F.);
#4429=ORIENTED_EDGE('',*,*,#3601,.F.);
#4430=ORIENTED_EDGE('',*,*,#3602,.T.);
#4431=ORIENTED_EDGE('',*,*,#3601,.T.);
#4432=ORIENTED_EDGE('',*,*,#3603,.F.);
#4433=ORIENTED_EDGE('',*,*,#3604,.F.);
#4434=ORIENTED_EDGE('',*,*,#3605,.T.);
#4435=ORIENTED_EDGE('',*,*,#3604,.T.);
#4436=ORIENTED_EDGE('',*,*,#3606,.F.);
#4437=ORIENTED_EDGE('',*,*,#3607,.F.);
#4438=ORIENTED_EDGE('',*,*,#3608,.T.);
#4439=ORIENTED_EDGE('',*,*,#3607,.T.);
#4440=ORIENTED_EDGE('',*,*,#3609,.F.);
#4441=ORIENTED_EDGE('',*,*,#3599,.F.);
#4442=ORIENTED_EDGE('',*,*,#3609,.T.);
#4443=ORIENTED_EDGE('',*,*,#3606,.T.);
#4444=ORIENTED_EDGE('',*,*,#3603,.T.);
#4445=ORIENTED_EDGE('',*,*,#3600,.T.);
#4446=ORIENTED_EDGE('',*,*,#3608,.F.);
#4447=ORIENTED_EDGE('',*,*,#3598,.F.);
#4448=ORIENTED_EDGE('',*,*,#3602,.F.);
#4449=ORIENTED_EDGE('',*,*,#3605,.F.);
#4450=ORIENTED_EDGE('',*,*,#3610,.T.);
#4451=ORIENTED_EDGE('',*,*,#3611,.T.);
#4452=ORIENTED_EDGE('',*,*,#3612,.F.);
#4453=ORIENTED_EDGE('',*,*,#3613,.F.);
#4454=ORIENTED_EDGE('',*,*,#3614,.T.);
#4455=ORIENTED_EDGE('',*,*,#3613,.T.);
#4456=ORIENTED_EDGE('',*,*,#3615,.F.);
#4457=ORIENTED_EDGE('',*,*,#3616,.F.);
#4458=ORIENTED_EDGE('',*,*,#3617,.T.);
#4459=ORIENTED_EDGE('',*,*,#3616,.T.);
#4460=ORIENTED_EDGE('',*,*,#3618,.F.);
#4461=ORIENTED_EDGE('',*,*,#3619,.F.);
#4462=ORIENTED_EDGE('',*,*,#3620,.T.);
#4463=ORIENTED_EDGE('',*,*,#3619,.T.);
#4464=ORIENTED_EDGE('',*,*,#3621,.F.);
#4465=ORIENTED_EDGE('',*,*,#3611,.F.);
#4466=ORIENTED_EDGE('',*,*,#3621,.T.);
#4467=ORIENTED_EDGE('',*,*,#3618,.T.);
#4468=ORIENTED_EDGE('',*,*,#3615,.T.);
#4469=ORIENTED_EDGE('',*,*,#3612,.T.);
#4470=ORIENTED_EDGE('',*,*,#3620,.F.);
#4471=ORIENTED_EDGE('',*,*,#3610,.F.);
#4472=ORIENTED_EDGE('',*,*,#3614,.F.);
#4473=ORIENTED_EDGE('',*,*,#3617,.F.);
#4474=ORIENTED_EDGE('',*,*,#3622,.T.);
#4475=ORIENTED_EDGE('',*,*,#3623,.T.);
#4476=ORIENTED_EDGE('',*,*,#3624,.F.);
#4477=ORIENTED_EDGE('',*,*,#3625,.F.);
#4478=ORIENTED_EDGE('',*,*,#3626,.T.);
#4479=ORIENTED_EDGE('',*,*,#3625,.T.);
#4480=ORIENTED_EDGE('',*,*,#3627,.F.);
#4481=ORIENTED_EDGE('',*,*,#3628,.F.);
#4482=ORIENTED_EDGE('',*,*,#3629,.T.);
#4483=ORIENTED_EDGE('',*,*,#3628,.T.);
#4484=ORIENTED_EDGE('',*,*,#3630,.F.);
#4485=ORIENTED_EDGE('',*,*,#3631,.F.);
#4486=ORIENTED_EDGE('',*,*,#3632,.T.);
#4487=ORIENTED_EDGE('',*,*,#3631,.T.);
#4488=ORIENTED_EDGE('',*,*,#3633,.F.);
#4489=ORIENTED_EDGE('',*,*,#3623,.F.);
#4490=ORIENTED_EDGE('',*,*,#3633,.T.);
#4491=ORIENTED_EDGE('',*,*,#3630,.T.);
#4492=ORIENTED_EDGE('',*,*,#3627,.T.);
#4493=ORIENTED_EDGE('',*,*,#3624,.T.);
#4494=ORIENTED_EDGE('',*,*,#3632,.F.);
#4495=ORIENTED_EDGE('',*,*,#3622,.F.);
#4496=ORIENTED_EDGE('',*,*,#3626,.F.);
#4497=ORIENTED_EDGE('',*,*,#3629,.F.);
#4498=ORIENTED_EDGE('',*,*,#3634,.T.);
#4499=ORIENTED_EDGE('',*,*,#3635,.T.);
#4500=ORIENTED_EDGE('',*,*,#3636,.F.);
#4501=ORIENTED_EDGE('',*,*,#3637,.F.);
#4502=ORIENTED_EDGE('',*,*,#3638,.T.);
#4503=ORIENTED_EDGE('',*,*,#3637,.T.);
#4504=ORIENTED_EDGE('',*,*,#3639,.F.);
#4505=ORIENTED_EDGE('',*,*,#3640,.F.);
#4506=ORIENTED_EDGE('',*,*,#3641,.T.);
#4507=ORIENTED_EDGE('',*,*,#3640,.T.);
#4508=ORIENTED_EDGE('',*,*,#3642,.F.);
#4509=ORIENTED_EDGE('',*,*,#3643,.F.);
#4510=ORIENTED_EDGE('',*,*,#3644,.T.);
#4511=ORIENTED_EDGE('',*,*,#3643,.T.);
#4512=ORIENTED_EDGE('',*,*,#3645,.F.);
#4513=ORIENTED_EDGE('',*,*,#3635,.F.);
#4514=ORIENTED_EDGE('',*,*,#3645,.T.);
#4515=ORIENTED_EDGE('',*,*,#3642,.T.);
#4516=ORIENTED_EDGE('',*,*,#3639,.T.);
#4517=ORIENTED_EDGE('',*,*,#3636,.T.);
#4518=ORIENTED_EDGE('',*,*,#3644,.F.);
#4519=ORIENTED_EDGE('',*,*,#3634,.F.);
#4520=ORIENTED_EDGE('',*,*,#3638,.F.);
#4521=ORIENTED_EDGE('',*,*,#3641,.F.);
#4522=ORIENTED_EDGE('',*,*,#3646,.F.);
#4523=ORIENTED_EDGE('',*,*,#3647,.T.);
#4524=ORIENTED_EDGE('',*,*,#3648,.F.);
#4525=ORIENTED_EDGE('',*,*,#3647,.F.);
#4526=ORIENTED_EDGE('',*,*,#3649,.F.);
#4527=ORIENTED_EDGE('',*,*,#3650,.T.);
#4528=ORIENTED_EDGE('',*,*,#3651,.F.);
#4529=ORIENTED_EDGE('',*,*,#3650,.F.);
#4530=ORIENTED_EDGE('',*,*,#3652,.F.);
#4531=ORIENTED_EDGE('',*,*,#3653,.T.);
#4532=ORIENTED_EDGE('',*,*,#3654,.F.);
#4533=ORIENTED_EDGE('',*,*,#3653,.F.);
#4534=ORIENTED_EDGE('',*,*,#3655,.F.);
#4535=ORIENTED_EDGE('',*,*,#3656,.T.);
#4536=ORIENTED_EDGE('',*,*,#3657,.F.);
#4537=ORIENTED_EDGE('',*,*,#3656,.F.);
#4538=ORIENTED_EDGE('',*,*,#3658,.F.);
#4539=ORIENTED_EDGE('',*,*,#3659,.T.);
#4540=ORIENTED_EDGE('',*,*,#3660,.F.);
#4541=ORIENTED_EDGE('',*,*,#3659,.F.);
#4542=ORIENTED_EDGE('',*,*,#3661,.F.);
#4543=ORIENTED_EDGE('',*,*,#3662,.T.);
#4544=ORIENTED_EDGE('',*,*,#3663,.F.);
#4545=ORIENTED_EDGE('',*,*,#3662,.F.);
#4546=ORIENTED_EDGE('',*,*,#3664,.F.);
#4547=ORIENTED_EDGE('',*,*,#3665,.T.);
#4548=ORIENTED_EDGE('',*,*,#3666,.F.);
#4549=ORIENTED_EDGE('',*,*,#3665,.F.);
#4550=ORIENTED_EDGE('',*,*,#3667,.F.);
#4551=ORIENTED_EDGE('',*,*,#3668,.F.);
#4552=ORIENTED_EDGE('',*,*,#3669,.F.);
#4553=ORIENTED_EDGE('',*,*,#3670,.T.);
#4554=ORIENTED_EDGE('',*,*,#3648,.T.);
#4555=ORIENTED_EDGE('',*,*,#3651,.T.);
#4556=ORIENTED_EDGE('',*,*,#3669,.T.);
#4557=ORIENTED_EDGE('',*,*,#3671,.T.);
#4558=ORIENTED_EDGE('',*,*,#3672,.T.);
#4559=ORIENTED_EDGE('',*,*,#3673,.T.);
#4560=ORIENTED_EDGE('',*,*,#3674,.T.);
#4561=ORIENTED_EDGE('',*,*,#3675,.F.);
#4562=ORIENTED_EDGE('',*,*,#3676,.F.);
#4563=ORIENTED_EDGE('',*,*,#3677,.T.);
#4564=ORIENTED_EDGE('',*,*,#3666,.T.);
#4565=ORIENTED_EDGE('',*,*,#3663,.T.);
#4566=ORIENTED_EDGE('',*,*,#3660,.T.);
#4567=ORIENTED_EDGE('',*,*,#3657,.T.);
#4568=ORIENTED_EDGE('',*,*,#3654,.T.);
#4569=ORIENTED_EDGE('',*,*,#3678,.T.);
#4570=ORIENTED_EDGE('',*,*,#3679,.F.);
#4571=ORIENTED_EDGE('',*,*,#3674,.F.);
#4572=ORIENTED_EDGE('',*,*,#3680,.T.);
#4573=ORIENTED_EDGE('',*,*,#3671,.F.);
#4574=ORIENTED_EDGE('',*,*,#3668,.T.);
#4575=ORIENTED_EDGE('',*,*,#3676,.T.);
#4576=ORIENTED_EDGE('',*,*,#3681,.F.);
#4577=ORIENTED_EDGE('',*,*,#3682,.F.);
#4578=ORIENTED_EDGE('',*,*,#3670,.F.);
#4579=ORIENTED_EDGE('',*,*,#3673,.F.);
#4580=ORIENTED_EDGE('',*,*,#3683,.T.);
#4581=ORIENTED_EDGE('',*,*,#3667,.T.);
#4582=ORIENTED_EDGE('',*,*,#3682,.T.);
#4583=ORIENTED_EDGE('',*,*,#3684,.F.);
#4584=ORIENTED_EDGE('',*,*,#3678,.F.);
#4585=ORIENTED_EDGE('',*,*,#3664,.T.);
#4586=ORIENTED_EDGE('',*,*,#3661,.T.);
#4587=ORIENTED_EDGE('',*,*,#3658,.T.);
#4588=ORIENTED_EDGE('',*,*,#3655,.T.);
#4589=ORIENTED_EDGE('',*,*,#3652,.T.);
#4590=ORIENTED_EDGE('',*,*,#3679,.T.);
#4591=ORIENTED_EDGE('',*,*,#3684,.T.);
#4592=ORIENTED_EDGE('',*,*,#3681,.T.);
#4593=ORIENTED_EDGE('',*,*,#3675,.T.);
#4594=ORIENTED_EDGE('',*,*,#3680,.F.);
#4595=ORIENTED_EDGE('',*,*,#3677,.F.);
#4596=ORIENTED_EDGE('',*,*,#3683,.F.);
#4597=ORIENTED_EDGE('',*,*,#3672,.F.);
#4598=ORIENTED_EDGE('',*,*,#3646,.T.);
#4599=ORIENTED_EDGE('',*,*,#3649,.T.);
#4600=ORIENTED_EDGE('',*,*,#3685,.F.);
#4601=ORIENTED_EDGE('',*,*,#3686,.T.);
#4602=ORIENTED_EDGE('',*,*,#3687,.T.);
#4603=ORIENTED_EDGE('',*,*,#3686,.F.);
#4604=ORIENTED_EDGE('',*,*,#3688,.F.);
#4605=ORIENTED_EDGE('',*,*,#3689,.T.);
#4606=ORIENTED_EDGE('',*,*,#3690,.T.);
#4607=ORIENTED_EDGE('',*,*,#3689,.F.);
#4608=ORIENTED_EDGE('',*,*,#3688,.T.);
#4609=ORIENTED_EDGE('',*,*,#3685,.T.);
#4610=ORIENTED_EDGE('',*,*,#3690,.F.);
#4611=ORIENTED_EDGE('',*,*,#3687,.F.);
#4612=ORIENTED_EDGE('',*,*,#3691,.F.);
#4613=ORIENTED_EDGE('',*,*,#3692,.T.);
#4614=ORIENTED_EDGE('',*,*,#3693,.T.);
#4615=ORIENTED_EDGE('',*,*,#3692,.F.);
#4616=ORIENTED_EDGE('',*,*,#3694,.F.);
#4617=ORIENTED_EDGE('',*,*,#3695,.T.);
#4618=ORIENTED_EDGE('',*,*,#3696,.T.);
#4619=ORIENTED_EDGE('',*,*,#3695,.F.);
#4620=ORIENTED_EDGE('',*,*,#3694,.T.);
#4621=ORIENTED_EDGE('',*,*,#3691,.T.);
#4622=ORIENTED_EDGE('',*,*,#3696,.F.);
#4623=ORIENTED_EDGE('',*,*,#3693,.F.);
#4624=ORIENTED_EDGE('',*,*,#3697,.F.);
#4625=ORIENTED_EDGE('',*,*,#3698,.T.);
#4626=ORIENTED_EDGE('',*,*,#3699,.T.);
#4627=ORIENTED_EDGE('',*,*,#3698,.F.);
#4628=ORIENTED_EDGE('',*,*,#3700,.F.);
#4629=ORIENTED_EDGE('',*,*,#3701,.T.);
#4630=ORIENTED_EDGE('',*,*,#3702,.T.);
#4631=ORIENTED_EDGE('',*,*,#3701,.F.);
#4632=ORIENTED_EDGE('',*,*,#3700,.T.);
#4633=ORIENTED_EDGE('',*,*,#3697,.T.);
#4634=ORIENTED_EDGE('',*,*,#3702,.F.);
#4635=ORIENTED_EDGE('',*,*,#3699,.F.);
#4636=ORIENTED_EDGE('',*,*,#3703,.F.);
#4637=ORIENTED_EDGE('',*,*,#3704,.T.);
#4638=ORIENTED_EDGE('',*,*,#3705,.T.);
#4639=ORIENTED_EDGE('',*,*,#3704,.F.);
#4640=ORIENTED_EDGE('',*,*,#3706,.F.);
#4641=ORIENTED_EDGE('',*,*,#3707,.T.);
#4642=ORIENTED_EDGE('',*,*,#3708,.T.);
#4643=ORIENTED_EDGE('',*,*,#3707,.F.);
#4644=ORIENTED_EDGE('',*,*,#3706,.T.);
#4645=ORIENTED_EDGE('',*,*,#3703,.T.);
#4646=ORIENTED_EDGE('',*,*,#3708,.F.);
#4647=ORIENTED_EDGE('',*,*,#3705,.F.);
#4648=ORIENTED_EDGE('',*,*,#3709,.F.);
#4649=ORIENTED_EDGE('',*,*,#3710,.T.);
#4650=ORIENTED_EDGE('',*,*,#3711,.F.);
#4651=ORIENTED_EDGE('',*,*,#3710,.F.);
#4652=ORIENTED_EDGE('',*,*,#3712,.F.);
#4653=ORIENTED_EDGE('',*,*,#3713,.T.);
#4654=ORIENTED_EDGE('',*,*,#3714,.F.);
#4655=ORIENTED_EDGE('',*,*,#3713,.F.);
#4656=ORIENTED_EDGE('',*,*,#3715,.F.);
#4657=ORIENTED_EDGE('',*,*,#3716,.T.);
#4658=ORIENTED_EDGE('',*,*,#3717,.F.);
#4659=ORIENTED_EDGE('',*,*,#3716,.F.);
#4660=ORIENTED_EDGE('',*,*,#3718,.F.);
#4661=ORIENTED_EDGE('',*,*,#3719,.T.);
#4662=ORIENTED_EDGE('',*,*,#3720,.F.);
#4663=ORIENTED_EDGE('',*,*,#3719,.F.);
#4664=ORIENTED_EDGE('',*,*,#3721,.F.);
#4665=ORIENTED_EDGE('',*,*,#3722,.T.);
#4666=ORIENTED_EDGE('',*,*,#3723,.F.);
#4667=ORIENTED_EDGE('',*,*,#3722,.F.);
#4668=ORIENTED_EDGE('',*,*,#3724,.F.);
#4669=ORIENTED_EDGE('',*,*,#3725,.T.);
#4670=ORIENTED_EDGE('',*,*,#3726,.F.);
#4671=ORIENTED_EDGE('',*,*,#3725,.F.);
#4672=ORIENTED_EDGE('',*,*,#3727,.F.);
#4673=ORIENTED_EDGE('',*,*,#3728,.T.);
#4674=ORIENTED_EDGE('',*,*,#3729,.F.);
#4675=ORIENTED_EDGE('',*,*,#3728,.F.);
#4676=ORIENTED_EDGE('',*,*,#3730,.F.);
#4677=ORIENTED_EDGE('',*,*,#3731,.F.);
#4678=ORIENTED_EDGE('',*,*,#3732,.F.);
#4679=ORIENTED_EDGE('',*,*,#3733,.T.);
#4680=ORIENTED_EDGE('',*,*,#3711,.T.);
#4681=ORIENTED_EDGE('',*,*,#3714,.T.);
#4682=ORIENTED_EDGE('',*,*,#3732,.T.);
#4683=ORIENTED_EDGE('',*,*,#3734,.T.);
#4684=ORIENTED_EDGE('',*,*,#3735,.T.);
#4685=ORIENTED_EDGE('',*,*,#3736,.T.);
#4686=ORIENTED_EDGE('',*,*,#3737,.T.);
#4687=ORIENTED_EDGE('',*,*,#3738,.F.);
#4688=ORIENTED_EDGE('',*,*,#3739,.F.);
#4689=ORIENTED_EDGE('',*,*,#3740,.T.);
#4690=ORIENTED_EDGE('',*,*,#3729,.T.);
#4691=ORIENTED_EDGE('',*,*,#3726,.T.);
#4692=ORIENTED_EDGE('',*,*,#3723,.T.);
#4693=ORIENTED_EDGE('',*,*,#3720,.T.);
#4694=ORIENTED_EDGE('',*,*,#3717,.T.);
#4695=ORIENTED_EDGE('',*,*,#3741,.T.);
#4696=ORIENTED_EDGE('',*,*,#3742,.F.);
#4697=ORIENTED_EDGE('',*,*,#3737,.F.);
#4698=ORIENTED_EDGE('',*,*,#3743,.T.);
#4699=ORIENTED_EDGE('',*,*,#3734,.F.);
#4700=ORIENTED_EDGE('',*,*,#3731,.T.);
#4701=ORIENTED_EDGE('',*,*,#3739,.T.);
#4702=ORIENTED_EDGE('',*,*,#3744,.F.);
#4703=ORIENTED_EDGE('',*,*,#3745,.F.);
#4704=ORIENTED_EDGE('',*,*,#3733,.F.);
#4705=ORIENTED_EDGE('',*,*,#3736,.F.);
#4706=ORIENTED_EDGE('',*,*,#3746,.T.);
#4707=ORIENTED_EDGE('',*,*,#3730,.T.);
#4708=ORIENTED_EDGE('',*,*,#3745,.T.);
#4709=ORIENTED_EDGE('',*,*,#3747,.F.);
#4710=ORIENTED_EDGE('',*,*,#3741,.F.);
#4711=ORIENTED_EDGE('',*,*,#3727,.T.);
#4712=ORIENTED_EDGE('',*,*,#3724,.T.);
#4713=ORIENTED_EDGE('',*,*,#3721,.T.);
#4714=ORIENTED_EDGE('',*,*,#3718,.T.);
#4715=ORIENTED_EDGE('',*,*,#3715,.T.);
#4716=ORIENTED_EDGE('',*,*,#3742,.T.);
#4717=ORIENTED_EDGE('',*,*,#3747,.T.);
#4718=ORIENTED_EDGE('',*,*,#3744,.T.);
#4719=ORIENTED_EDGE('',*,*,#3738,.T.);
#4720=ORIENTED_EDGE('',*,*,#3743,.F.);
#4721=ORIENTED_EDGE('',*,*,#3740,.F.);
#4722=ORIENTED_EDGE('',*,*,#3746,.F.);
#4723=ORIENTED_EDGE('',*,*,#3735,.F.);
#4724=ORIENTED_EDGE('',*,*,#3709,.T.);
#4725=ORIENTED_EDGE('',*,*,#3712,.T.);
#4726=ORIENTED_EDGE('',*,*,#3748,.F.);
#4727=ORIENTED_EDGE('',*,*,#3749,.T.);
#4728=ORIENTED_EDGE('',*,*,#3750,.T.);
#4729=ORIENTED_EDGE('',*,*,#3749,.F.);
#4730=ORIENTED_EDGE('',*,*,#3751,.F.);
#4731=ORIENTED_EDGE('',*,*,#3752,.T.);
#4732=ORIENTED_EDGE('',*,*,#3753,.T.);
#4733=ORIENTED_EDGE('',*,*,#3752,.F.);
#4734=ORIENTED_EDGE('',*,*,#3751,.T.);
#4735=ORIENTED_EDGE('',*,*,#3748,.T.);
#4736=ORIENTED_EDGE('',*,*,#3753,.F.);
#4737=ORIENTED_EDGE('',*,*,#3750,.F.);
#4738=ORIENTED_EDGE('',*,*,#3754,.F.);
#4739=ORIENTED_EDGE('',*,*,#3755,.T.);
#4740=ORIENTED_EDGE('',*,*,#3756,.T.);
#4741=ORIENTED_EDGE('',*,*,#3755,.F.);
#4742=ORIENTED_EDGE('',*,*,#3757,.F.);
#4743=ORIENTED_EDGE('',*,*,#3758,.T.);
#4744=ORIENTED_EDGE('',*,*,#3759,.T.);
#4745=ORIENTED_EDGE('',*,*,#3758,.F.);
#4746=ORIENTED_EDGE('',*,*,#3757,.T.);
#4747=ORIENTED_EDGE('',*,*,#3754,.T.);
#4748=ORIENTED_EDGE('',*,*,#3759,.F.);
#4749=ORIENTED_EDGE('',*,*,#3756,.F.);
#4750=ORIENTED_EDGE('',*,*,#3760,.F.);
#4751=ORIENTED_EDGE('',*,*,#3761,.T.);
#4752=ORIENTED_EDGE('',*,*,#3762,.T.);
#4753=ORIENTED_EDGE('',*,*,#3761,.F.);
#4754=ORIENTED_EDGE('',*,*,#3763,.F.);
#4755=ORIENTED_EDGE('',*,*,#3764,.T.);
#4756=ORIENTED_EDGE('',*,*,#3765,.T.);
#4757=ORIENTED_EDGE('',*,*,#3764,.F.);
#4758=ORIENTED_EDGE('',*,*,#3763,.T.);
#4759=ORIENTED_EDGE('',*,*,#3760,.T.);
#4760=ORIENTED_EDGE('',*,*,#3765,.F.);
#4761=ORIENTED_EDGE('',*,*,#3762,.F.);
#4762=ORIENTED_EDGE('',*,*,#3766,.F.);
#4763=ORIENTED_EDGE('',*,*,#3767,.T.);
#4764=ORIENTED_EDGE('',*,*,#3768,.T.);
#4765=ORIENTED_EDGE('',*,*,#3767,.F.);
#4766=ORIENTED_EDGE('',*,*,#3769,.F.);
#4767=ORIENTED_EDGE('',*,*,#3770,.T.);
#4768=ORIENTED_EDGE('',*,*,#3771,.T.);
#4769=ORIENTED_EDGE('',*,*,#3770,.F.);
#4770=ORIENTED_EDGE('',*,*,#3769,.T.);
#4771=ORIENTED_EDGE('',*,*,#3766,.T.);
#4772=ORIENTED_EDGE('',*,*,#3771,.F.);
#4773=ORIENTED_EDGE('',*,*,#3768,.F.);
#4774=ORIENTED_EDGE('',*,*,#3772,.F.);
#4775=ORIENTED_EDGE('',*,*,#3773,.T.);
#4776=ORIENTED_EDGE('',*,*,#3774,.F.);
#4777=ORIENTED_EDGE('',*,*,#3775,.F.);
#4778=ORIENTED_EDGE('',*,*,#3776,.F.);
#4779=ORIENTED_EDGE('',*,*,#3777,.T.);
#4780=ORIENTED_EDGE('',*,*,#3778,.F.);
#4781=ORIENTED_EDGE('',*,*,#3773,.F.);
#4782=ORIENTED_EDGE('',*,*,#3779,.F.);
#4783=ORIENTED_EDGE('',*,*,#3780,.T.);
#4784=ORIENTED_EDGE('',*,*,#3781,.F.);
#4785=ORIENTED_EDGE('',*,*,#3777,.F.);
#4786=ORIENTED_EDGE('',*,*,#3782,.F.);
#4787=ORIENTED_EDGE('',*,*,#3783,.T.);
#4788=ORIENTED_EDGE('',*,*,#3784,.F.);
#4789=ORIENTED_EDGE('',*,*,#3780,.F.);
#4790=ORIENTED_EDGE('',*,*,#3785,.F.);
#4791=ORIENTED_EDGE('',*,*,#3786,.T.);
#4792=ORIENTED_EDGE('',*,*,#3787,.F.);
#4793=ORIENTED_EDGE('',*,*,#3783,.F.);
#4794=ORIENTED_EDGE('',*,*,#3788,.F.);
#4795=ORIENTED_EDGE('',*,*,#3789,.T.);
#4796=ORIENTED_EDGE('',*,*,#3790,.F.);
#4797=ORIENTED_EDGE('',*,*,#3786,.F.);
#4798=ORIENTED_EDGE('',*,*,#3791,.F.);
#4799=ORIENTED_EDGE('',*,*,#3792,.T.);
#4800=ORIENTED_EDGE('',*,*,#3793,.F.);
#4801=ORIENTED_EDGE('',*,*,#3789,.F.);
#4802=ORIENTED_EDGE('',*,*,#3794,.F.);
#4803=ORIENTED_EDGE('',*,*,#3795,.T.);
#4804=ORIENTED_EDGE('',*,*,#3796,.F.);
#4805=ORIENTED_EDGE('',*,*,#3792,.F.);
#4806=ORIENTED_EDGE('',*,*,#3797,.F.);
#4807=ORIENTED_EDGE('',*,*,#3798,.F.);
#4808=ORIENTED_EDGE('',*,*,#3799,.F.);
#4809=ORIENTED_EDGE('',*,*,#3795,.F.);
#4810=ORIENTED_EDGE('',*,*,#3800,.F.);
#4811=ORIENTED_EDGE('',*,*,#3801,.T.);
#4812=ORIENTED_EDGE('',*,*,#3802,.F.);
#4813=ORIENTED_EDGE('',*,*,#3803,.F.);
#4814=ORIENTED_EDGE('',*,*,#3804,.F.);
#4815=ORIENTED_EDGE('',*,*,#3805,.T.);
#4816=ORIENTED_EDGE('',*,*,#3806,.F.);
#4817=ORIENTED_EDGE('',*,*,#3801,.F.);
#4818=ORIENTED_EDGE('',*,*,#3807,.F.);
#4819=ORIENTED_EDGE('',*,*,#3808,.T.);
#4820=ORIENTED_EDGE('',*,*,#3809,.F.);
#4821=ORIENTED_EDGE('',*,*,#3805,.F.);
#4822=ORIENTED_EDGE('',*,*,#3810,.F.);
#4823=ORIENTED_EDGE('',*,*,#3811,.T.);
#4824=ORIENTED_EDGE('',*,*,#3812,.F.);
#4825=ORIENTED_EDGE('',*,*,#3808,.F.);
#4826=ORIENTED_EDGE('',*,*,#3813,.F.);
#4827=ORIENTED_EDGE('',*,*,#3814,.T.);
#4828=ORIENTED_EDGE('',*,*,#3815,.F.);
#4829=ORIENTED_EDGE('',*,*,#3811,.F.);
#4830=ORIENTED_EDGE('',*,*,#3816,.F.);
#4831=ORIENTED_EDGE('',*,*,#3817,.T.);
#4832=ORIENTED_EDGE('',*,*,#3818,.F.);
#4833=ORIENTED_EDGE('',*,*,#3814,.F.);
#4834=ORIENTED_EDGE('',*,*,#3819,.F.);
#4835=ORIENTED_EDGE('',*,*,#3820,.T.);
#4836=ORIENTED_EDGE('',*,*,#3821,.F.);
#4837=ORIENTED_EDGE('',*,*,#3817,.F.);
#4838=ORIENTED_EDGE('',*,*,#3822,.F.);
#4839=ORIENTED_EDGE('',*,*,#3823,.T.);
#4840=ORIENTED_EDGE('',*,*,#3824,.F.);
#4841=ORIENTED_EDGE('',*,*,#3820,.F.);
#4842=ORIENTED_EDGE('',*,*,#3825,.F.);
#4843=ORIENTED_EDGE('',*,*,#3826,.F.);
#4844=ORIENTED_EDGE('',*,*,#3827,.F.);
#4845=ORIENTED_EDGE('',*,*,#3823,.F.);
#4846=ORIENTED_EDGE('',*,*,#3828,.F.);
#4847=ORIENTED_EDGE('',*,*,#3829,.T.);
#4848=ORIENTED_EDGE('',*,*,#3830,.F.);
#4849=ORIENTED_EDGE('',*,*,#3831,.F.);
#4850=ORIENTED_EDGE('',*,*,#3832,.F.);
#4851=ORIENTED_EDGE('',*,*,#3833,.T.);
#4852=ORIENTED_EDGE('',*,*,#3834,.F.);
#4853=ORIENTED_EDGE('',*,*,#3829,.F.);
#4854=ORIENTED_EDGE('',*,*,#3835,.F.);
#4855=ORIENTED_EDGE('',*,*,#3836,.T.);
#4856=ORIENTED_EDGE('',*,*,#3837,.F.);
#4857=ORIENTED_EDGE('',*,*,#3833,.F.);
#4858=ORIENTED_EDGE('',*,*,#3838,.F.);
#4859=ORIENTED_EDGE('',*,*,#3839,.T.);
#4860=ORIENTED_EDGE('',*,*,#3840,.F.);
#4861=ORIENTED_EDGE('',*,*,#3836,.F.);
#4862=ORIENTED_EDGE('',*,*,#3841,.F.);
#4863=ORIENTED_EDGE('',*,*,#3842,.T.);
#4864=ORIENTED_EDGE('',*,*,#3843,.F.);
#4865=ORIENTED_EDGE('',*,*,#3839,.F.);
#4866=ORIENTED_EDGE('',*,*,#3844,.F.);
#4867=ORIENTED_EDGE('',*,*,#3845,.T.);
#4868=ORIENTED_EDGE('',*,*,#3846,.F.);
#4869=ORIENTED_EDGE('',*,*,#3842,.F.);
#4870=ORIENTED_EDGE('',*,*,#3847,.F.);
#4871=ORIENTED_EDGE('',*,*,#3848,.T.);
#4872=ORIENTED_EDGE('',*,*,#3849,.F.);
#4873=ORIENTED_EDGE('',*,*,#3845,.F.);
#4874=ORIENTED_EDGE('',*,*,#3850,.F.);
#4875=ORIENTED_EDGE('',*,*,#3851,.T.);
#4876=ORIENTED_EDGE('',*,*,#3852,.F.);
#4877=ORIENTED_EDGE('',*,*,#3848,.F.);
#4878=ORIENTED_EDGE('',*,*,#3853,.F.);
#4879=ORIENTED_EDGE('',*,*,#3854,.F.);
#4880=ORIENTED_EDGE('',*,*,#3855,.F.);
#4881=ORIENTED_EDGE('',*,*,#3851,.F.);
#4882=ORIENTED_EDGE('',*,*,#3856,.F.);
#4883=ORIENTED_EDGE('',*,*,#3857,.T.);
#4884=ORIENTED_EDGE('',*,*,#3858,.F.);
#4885=ORIENTED_EDGE('',*,*,#3859,.F.);
#4886=ORIENTED_EDGE('',*,*,#3860,.F.);
#4887=ORIENTED_EDGE('',*,*,#3861,.T.);
#4888=ORIENTED_EDGE('',*,*,#3862,.F.);
#4889=ORIENTED_EDGE('',*,*,#3857,.F.);
#4890=ORIENTED_EDGE('',*,*,#3863,.F.);
#4891=ORIENTED_EDGE('',*,*,#3864,.T.);
#4892=ORIENTED_EDGE('',*,*,#3865,.F.);
#4893=ORIENTED_EDGE('',*,*,#3861,.F.);
#4894=ORIENTED_EDGE('',*,*,#3866,.F.);
#4895=ORIENTED_EDGE('',*,*,#3867,.T.);
#4896=ORIENTED_EDGE('',*,*,#3868,.F.);
#4897=ORIENTED_EDGE('',*,*,#3864,.F.);
#4898=ORIENTED_EDGE('',*,*,#3869,.F.);
#4899=ORIENTED_EDGE('',*,*,#3870,.T.);
#4900=ORIENTED_EDGE('',*,*,#3871,.F.);
#4901=ORIENTED_EDGE('',*,*,#3867,.F.);
#4902=ORIENTED_EDGE('',*,*,#3872,.F.);
#4903=ORIENTED_EDGE('',*,*,#3873,.T.);
#4904=ORIENTED_EDGE('',*,*,#3874,.F.);
#4905=ORIENTED_EDGE('',*,*,#3870,.F.);
#4906=ORIENTED_EDGE('',*,*,#3875,.F.);
#4907=ORIENTED_EDGE('',*,*,#3876,.T.);
#4908=ORIENTED_EDGE('',*,*,#3877,.F.);
#4909=ORIENTED_EDGE('',*,*,#3873,.F.);
#4910=ORIENTED_EDGE('',*,*,#3878,.F.);
#4911=ORIENTED_EDGE('',*,*,#3879,.T.);
#4912=ORIENTED_EDGE('',*,*,#3880,.F.);
#4913=ORIENTED_EDGE('',*,*,#3876,.F.);
#4914=ORIENTED_EDGE('',*,*,#3881,.F.);
#4915=ORIENTED_EDGE('',*,*,#3882,.F.);
#4916=ORIENTED_EDGE('',*,*,#3883,.F.);
#4917=ORIENTED_EDGE('',*,*,#3879,.F.);
#4918=ORIENTED_EDGE('',*,*,#3884,.F.);
#4919=ORIENTED_EDGE('',*,*,#3885,.T.);
#4920=ORIENTED_EDGE('',*,*,#3886,.F.);
#4921=ORIENTED_EDGE('',*,*,#3885,.F.);
#4922=ORIENTED_EDGE('',*,*,#3798,.T.);
#4923=ORIENTED_EDGE('',*,*,#3887,.T.);
#4924=ORIENTED_EDGE('',*,*,#3888,.T.);
#4925=ORIENTED_EDGE('',*,*,#3889,.F.);
#4926=ORIENTED_EDGE('',*,*,#3775,.T.);
#4927=ORIENTED_EDGE('',*,*,#3890,.F.);
#4928=ORIENTED_EDGE('',*,*,#3891,.F.);
#4929=ORIENTED_EDGE('',*,*,#3892,.T.);
#4930=ORIENTED_EDGE('',*,*,#3826,.T.);
#4931=ORIENTED_EDGE('',*,*,#3893,.T.);
#4932=ORIENTED_EDGE('',*,*,#3891,.T.);
#4933=ORIENTED_EDGE('',*,*,#3894,.F.);
#4934=ORIENTED_EDGE('',*,*,#3803,.T.);
#4935=ORIENTED_EDGE('',*,*,#3895,.F.);
#4936=ORIENTED_EDGE('',*,*,#3896,.F.);
#4937=ORIENTED_EDGE('',*,*,#3897,.T.);
#4938=ORIENTED_EDGE('',*,*,#3854,.T.);
#4939=ORIENTED_EDGE('',*,*,#3898,.T.);
#4940=ORIENTED_EDGE('',*,*,#3896,.T.);
#4941=ORIENTED_EDGE('',*,*,#3899,.F.);
#4942=ORIENTED_EDGE('',*,*,#3831,.T.);
#4943=ORIENTED_EDGE('',*,*,#3900,.F.);
#4944=ORIENTED_EDGE('',*,*,#3901,.F.);
#4945=ORIENTED_EDGE('',*,*,#3902,.T.);
#4946=ORIENTED_EDGE('',*,*,#3882,.T.);
#4947=ORIENTED_EDGE('',*,*,#3903,.T.);
#4948=ORIENTED_EDGE('',*,*,#3901,.T.);
#4949=ORIENTED_EDGE('',*,*,#3904,.F.);
#4950=ORIENTED_EDGE('',*,*,#3859,.T.);
#4951=ORIENTED_EDGE('',*,*,#3905,.F.);
#4952=ORIENTED_EDGE('',*,*,#3888,.F.);
#4953=ORIENTED_EDGE('',*,*,#3906,.T.);
#4954=ORIENTED_EDGE('',*,*,#3774,.T.);
#4955=ORIENTED_EDGE('',*,*,#3778,.T.);
#4956=ORIENTED_EDGE('',*,*,#3781,.T.);
#4957=ORIENTED_EDGE('',*,*,#3784,.T.);
#4958=ORIENTED_EDGE('',*,*,#3787,.T.);
#4959=ORIENTED_EDGE('',*,*,#3790,.T.);
#4960=ORIENTED_EDGE('',*,*,#3793,.T.);
#4961=ORIENTED_EDGE('',*,*,#3796,.T.);
#4962=ORIENTED_EDGE('',*,*,#3799,.T.);
#4963=ORIENTED_EDGE('',*,*,#3889,.T.);
#4964=ORIENTED_EDGE('',*,*,#3905,.T.);
#4965=ORIENTED_EDGE('',*,*,#3858,.T.);
#4966=ORIENTED_EDGE('',*,*,#3862,.T.);
#4967=ORIENTED_EDGE('',*,*,#3865,.T.);
#4968=ORIENTED_EDGE('',*,*,#3868,.T.);
#4969=ORIENTED_EDGE('',*,*,#3871,.T.);
#4970=ORIENTED_EDGE('',*,*,#3874,.T.);
#4971=ORIENTED_EDGE('',*,*,#3877,.T.);
#4972=ORIENTED_EDGE('',*,*,#3880,.T.);
#4973=ORIENTED_EDGE('',*,*,#3883,.T.);
#4974=ORIENTED_EDGE('',*,*,#3904,.T.);
#4975=ORIENTED_EDGE('',*,*,#3900,.T.);
#4976=ORIENTED_EDGE('',*,*,#3830,.T.);
#4977=ORIENTED_EDGE('',*,*,#3834,.T.);
#4978=ORIENTED_EDGE('',*,*,#3837,.T.);
#4979=ORIENTED_EDGE('',*,*,#3840,.T.);
#4980=ORIENTED_EDGE('',*,*,#3843,.T.);
#4981=ORIENTED_EDGE('',*,*,#3846,.T.);
#4982=ORIENTED_EDGE('',*,*,#3849,.T.);
#4983=ORIENTED_EDGE('',*,*,#3852,.T.);
#4984=ORIENTED_EDGE('',*,*,#3855,.T.);
#4985=ORIENTED_EDGE('',*,*,#3899,.T.);
#4986=ORIENTED_EDGE('',*,*,#3895,.T.);
#4987=ORIENTED_EDGE('',*,*,#3802,.T.);
#4988=ORIENTED_EDGE('',*,*,#3806,.T.);
#4989=ORIENTED_EDGE('',*,*,#3809,.T.);
#4990=ORIENTED_EDGE('',*,*,#3812,.T.);
#4991=ORIENTED_EDGE('',*,*,#3815,.T.);
#4992=ORIENTED_EDGE('',*,*,#3818,.T.);
#4993=ORIENTED_EDGE('',*,*,#3821,.T.);
#4994=ORIENTED_EDGE('',*,*,#3824,.T.);
#4995=ORIENTED_EDGE('',*,*,#3827,.T.);
#4996=ORIENTED_EDGE('',*,*,#3894,.T.);
#4997=ORIENTED_EDGE('',*,*,#3890,.T.);
#4998=ORIENTED_EDGE('',*,*,#3886,.T.);
#4999=ORIENTED_EDGE('',*,*,#3772,.T.);
#5000=ORIENTED_EDGE('',*,*,#3892,.F.);
#5001=ORIENTED_EDGE('',*,*,#3893,.F.);
#5002=ORIENTED_EDGE('',*,*,#3825,.T.);
#5003=ORIENTED_EDGE('',*,*,#3822,.T.);
#5004=ORIENTED_EDGE('',*,*,#3819,.T.);
#5005=ORIENTED_EDGE('',*,*,#3816,.T.);
#5006=ORIENTED_EDGE('',*,*,#3813,.T.);
#5007=ORIENTED_EDGE('',*,*,#3810,.T.);
#5008=ORIENTED_EDGE('',*,*,#3807,.T.);
#5009=ORIENTED_EDGE('',*,*,#3804,.T.);
#5010=ORIENTED_EDGE('',*,*,#3800,.T.);
#5011=ORIENTED_EDGE('',*,*,#3897,.F.);
#5012=ORIENTED_EDGE('',*,*,#3898,.F.);
#5013=ORIENTED_EDGE('',*,*,#3853,.T.);
#5014=ORIENTED_EDGE('',*,*,#3850,.T.);
#5015=ORIENTED_EDGE('',*,*,#3847,.T.);
#5016=ORIENTED_EDGE('',*,*,#3844,.T.);
#5017=ORIENTED_EDGE('',*,*,#3841,.T.);
#5018=ORIENTED_EDGE('',*,*,#3838,.T.);
#5019=ORIENTED_EDGE('',*,*,#3835,.T.);
#5020=ORIENTED_EDGE('',*,*,#3832,.T.);
#5021=ORIENTED_EDGE('',*,*,#3828,.T.);
#5022=ORIENTED_EDGE('',*,*,#3902,.F.);
#5023=ORIENTED_EDGE('',*,*,#3903,.F.);
#5024=ORIENTED_EDGE('',*,*,#3881,.T.);
#5025=ORIENTED_EDGE('',*,*,#3878,.T.);
#5026=ORIENTED_EDGE('',*,*,#3875,.T.);
#5027=ORIENTED_EDGE('',*,*,#3872,.T.);
#5028=ORIENTED_EDGE('',*,*,#3869,.T.);
#5029=ORIENTED_EDGE('',*,*,#3866,.T.);
#5030=ORIENTED_EDGE('',*,*,#3863,.T.);
#5031=ORIENTED_EDGE('',*,*,#3860,.T.);
#5032=ORIENTED_EDGE('',*,*,#3856,.T.);
#5033=ORIENTED_EDGE('',*,*,#3906,.F.);
#5034=ORIENTED_EDGE('',*,*,#3887,.F.);
#5035=ORIENTED_EDGE('',*,*,#3797,.T.);
#5036=ORIENTED_EDGE('',*,*,#3794,.T.);
#5037=ORIENTED_EDGE('',*,*,#3791,.T.);
#5038=ORIENTED_EDGE('',*,*,#3788,.T.);
#5039=ORIENTED_EDGE('',*,*,#3785,.T.);
#5040=ORIENTED_EDGE('',*,*,#3782,.T.);
#5041=ORIENTED_EDGE('',*,*,#3779,.T.);
#5042=ORIENTED_EDGE('',*,*,#3776,.T.);
#5043=ORIENTED_EDGE('',*,*,#3884,.T.);
#5044=ORIENTED_EDGE('',*,*,#3907,.F.);
#5045=ORIENTED_EDGE('',*,*,#3908,.F.);
#5046=ORIENTED_EDGE('',*,*,#3909,.F.);
#5047=ORIENTED_EDGE('',*,*,#3910,.F.);
#5048=ORIENTED_EDGE('',*,*,#3909,.T.);
#5049=ORIENTED_EDGE('',*,*,#3911,.T.);
#5050=ORIENTED_EDGE('',*,*,#3912,.F.);
#5051=ORIENTED_EDGE('',*,*,#3913,.F.);
#5052=ORIENTED_EDGE('',*,*,#3914,.T.);
#5053=ORIENTED_EDGE('',*,*,#3915,.T.);
#5054=ORIENTED_EDGE('',*,*,#3916,.T.);
#5055=ORIENTED_EDGE('',*,*,#3912,.T.);
#5056=ORIENTED_EDGE('',*,*,#3917,.T.);
#5057=ORIENTED_EDGE('',*,*,#3914,.F.);
#5058=ORIENTED_EDGE('',*,*,#3911,.F.);
#5059=ORIENTED_EDGE('',*,*,#3908,.T.);
#5060=ORIENTED_EDGE('',*,*,#3918,.F.);
#5061=ORIENTED_EDGE('',*,*,#3919,.F.);
#5062=ORIENTED_EDGE('',*,*,#3920,.T.);
#5063=ORIENTED_EDGE('',*,*,#3921,.F.);
#5064=ORIENTED_EDGE('',*,*,#3922,.T.);
#5065=ORIENTED_EDGE('',*,*,#3923,.T.);
#5066=ORIENTED_EDGE('',*,*,#3924,.T.);
#5067=ORIENTED_EDGE('',*,*,#3925,.T.);
#5068=ORIENTED_EDGE('',*,*,#3926,.T.);
#5069=ORIENTED_EDGE('',*,*,#3915,.F.);
#5070=ORIENTED_EDGE('',*,*,#3924,.F.);
#5071=ORIENTED_EDGE('',*,*,#3927,.F.);
#5072=ORIENTED_EDGE('',*,*,#3928,.F.);
#5073=ORIENTED_EDGE('',*,*,#3925,.F.);
#5074=ORIENTED_EDGE('',*,*,#3923,.F.);
#5075=ORIENTED_EDGE('',*,*,#3916,.F.);
#5076=ORIENTED_EDGE('',*,*,#3926,.F.);
#5077=ORIENTED_EDGE('',*,*,#3928,.T.);
#5078=ORIENTED_EDGE('',*,*,#3929,.F.);
#5079=ORIENTED_EDGE('',*,*,#3930,.F.);
#5080=ORIENTED_EDGE('',*,*,#3931,.T.);
#5081=ORIENTED_EDGE('',*,*,#3932,.F.);
#5082=ORIENTED_EDGE('',*,*,#3933,.T.);
#5083=ORIENTED_EDGE('',*,*,#3910,.T.);
#5084=ORIENTED_EDGE('',*,*,#3913,.T.);
#5085=ORIENTED_EDGE('',*,*,#3927,.T.);
#5086=ORIENTED_EDGE('',*,*,#3922,.F.);
#5087=ORIENTED_EDGE('',*,*,#3934,.F.);
#5088=ORIENTED_EDGE('',*,*,#3929,.T.);
#5089=ORIENTED_EDGE('',*,*,#3930,.T.);
#5090=ORIENTED_EDGE('',*,*,#3934,.T.);
#5091=ORIENTED_EDGE('',*,*,#3921,.T.);
#5092=ORIENTED_EDGE('',*,*,#3935,.T.);
#5093=ORIENTED_EDGE('',*,*,#3936,.T.);
#5094=ORIENTED_EDGE('',*,*,#3937,.T.);
#5095=ORIENTED_EDGE('',*,*,#3936,.F.);
#5096=ORIENTED_EDGE('',*,*,#3938,.F.);
#5097=ORIENTED_EDGE('',*,*,#3939,.T.);
#5098=ORIENTED_EDGE('',*,*,#3917,.F.);
#5099=ORIENTED_EDGE('',*,*,#3939,.F.);
#5100=ORIENTED_EDGE('',*,*,#3940,.F.);
#5101=ORIENTED_EDGE('',*,*,#3941,.F.);
#5102=ORIENTED_EDGE('',*,*,#3942,.F.);
#5103=ORIENTED_EDGE('',*,*,#3935,.F.);
#5104=ORIENTED_EDGE('',*,*,#3920,.F.);
#5105=ORIENTED_EDGE('',*,*,#3943,.F.);
#5106=ORIENTED_EDGE('',*,*,#3940,.T.);
#5107=ORIENTED_EDGE('',*,*,#3938,.T.);
#5108=ORIENTED_EDGE('',*,*,#3937,.F.);
#5109=ORIENTED_EDGE('',*,*,#3942,.T.);
#5110=ORIENTED_EDGE('',*,*,#3944,.F.);
#5111=ORIENTED_EDGE('',*,*,#3931,.F.);
#5112=ORIENTED_EDGE('',*,*,#3919,.T.);
#5113=ORIENTED_EDGE('',*,*,#3945,.T.);
#5114=ORIENTED_EDGE('',*,*,#3932,.T.);
#5115=ORIENTED_EDGE('',*,*,#3944,.T.);
#5116=ORIENTED_EDGE('',*,*,#3941,.T.);
#5117=ORIENTED_EDGE('',*,*,#3943,.T.);
#5118=ORIENTED_EDGE('',*,*,#3907,.T.);
#5119=ORIENTED_EDGE('',*,*,#3933,.F.);
#5120=ORIENTED_EDGE('',*,*,#3945,.F.);
#5121=ORIENTED_EDGE('',*,*,#3918,.T.);
#5122=ORIENTED_EDGE('',*,*,#3946,.T.);
#5123=ORIENTED_EDGE('',*,*,#3947,.T.);
#5124=ORIENTED_EDGE('',*,*,#3948,.T.);
#5125=ORIENTED_EDGE('',*,*,#3949,.F.);
#5126=ORIENTED_EDGE('',*,*,#3950,.T.);
#5127=ORIENTED_EDGE('',*,*,#3951,.T.);
#5128=ORIENTED_EDGE('',*,*,#3952,.T.);
#5129=ORIENTED_EDGE('',*,*,#3947,.F.);
#5130=ORIENTED_EDGE('',*,*,#3953,.T.);
#5131=ORIENTED_EDGE('',*,*,#3954,.T.);
#5132=ORIENTED_EDGE('',*,*,#3955,.T.);
#5133=ORIENTED_EDGE('',*,*,#3951,.F.);
#5134=ORIENTED_EDGE('',*,*,#3956,.T.);
#5135=ORIENTED_EDGE('',*,*,#3957,.T.);
#5136=ORIENTED_EDGE('',*,*,#3958,.T.);
#5137=ORIENTED_EDGE('',*,*,#3954,.F.);
#5138=ORIENTED_EDGE('',*,*,#3959,.T.);
#5139=ORIENTED_EDGE('',*,*,#3960,.T.);
#5140=ORIENTED_EDGE('',*,*,#3961,.T.);
#5141=ORIENTED_EDGE('',*,*,#3957,.F.);
#5142=ORIENTED_EDGE('',*,*,#3962,.T.);
#5143=ORIENTED_EDGE('',*,*,#3949,.T.);
#5144=ORIENTED_EDGE('',*,*,#3963,.T.);
#5145=ORIENTED_EDGE('',*,*,#3960,.F.);
#5146=ORIENTED_EDGE('',*,*,#3962,.F.);
#5147=ORIENTED_EDGE('',*,*,#3959,.F.);
#5148=ORIENTED_EDGE('',*,*,#3956,.F.);
#5149=ORIENTED_EDGE('',*,*,#3953,.F.);
#5150=ORIENTED_EDGE('',*,*,#3950,.F.);
#5151=ORIENTED_EDGE('',*,*,#3946,.F.);
#5152=ORIENTED_EDGE('',*,*,#3963,.F.);
#5153=ORIENTED_EDGE('',*,*,#3948,.F.);
#5154=ORIENTED_EDGE('',*,*,#3952,.F.);
#5155=ORIENTED_EDGE('',*,*,#3955,.F.);
#5156=ORIENTED_EDGE('',*,*,#3958,.F.);
#5157=ORIENTED_EDGE('',*,*,#3961,.F.);
#5158=ORIENTED_EDGE('',*,*,#3964,.F.);
#5159=ORIENTED_EDGE('',*,*,#3965,.F.);
#5160=ORIENTED_EDGE('',*,*,#3966,.F.);
#5161=ORIENTED_EDGE('',*,*,#3967,.T.);
#5162=ORIENTED_EDGE('',*,*,#3965,.T.);
#5163=ORIENTED_EDGE('',*,*,#3967,.F.);
#5164=ORIENTED_EDGE('',*,*,#3968,.F.);
#5165=ORIENTED_EDGE('',*,*,#3969,.T.);
#5166=ORIENTED_EDGE('',*,*,#3966,.T.);
#5167=ORIENTED_EDGE('',*,*,#3969,.F.);
#5168=ORIENTED_EDGE('',*,*,#3970,.F.);
#5169=ORIENTED_EDGE('',*,*,#3971,.T.);
#5170=ORIENTED_EDGE('',*,*,#3968,.T.);
#5171=ORIENTED_EDGE('',*,*,#3971,.F.);
#5172=ORIENTED_EDGE('',*,*,#3970,.T.);
#5173=ORIENTED_EDGE('',*,*,#3972,.F.);
#5174=ORIENTED_EDGE('',*,*,#3973,.F.);
#5175=ORIENTED_EDGE('',*,*,#3974,.T.);
#5176=ORIENTED_EDGE('',*,*,#3972,.T.);
#5177=ORIENTED_EDGE('',*,*,#3974,.F.);
#5178=ORIENTED_EDGE('',*,*,#3964,.T.);
#5179=ORIENTED_EDGE('',*,*,#3975,.T.);
#5180=ORIENTED_EDGE('',*,*,#3973,.T.);
#5181=ORIENTED_EDGE('',*,*,#3975,.F.);
#5182=ORIENTED_EDGE('',*,*,#3976,.T.);
#5183=ORIENTED_EDGE('',*,*,#3977,.T.);
#5184=ORIENTED_EDGE('',*,*,#3978,.T.);
#5185=ORIENTED_EDGE('',*,*,#3979,.F.);
#5186=ORIENTED_EDGE('',*,*,#3980,.T.);
#5187=ORIENTED_EDGE('',*,*,#3981,.T.);
#5188=ORIENTED_EDGE('',*,*,#3982,.T.);
#5189=ORIENTED_EDGE('',*,*,#3977,.F.);
#5190=ORIENTED_EDGE('',*,*,#3983,.T.);
#5191=ORIENTED_EDGE('',*,*,#3984,.T.);
#5192=ORIENTED_EDGE('',*,*,#3985,.T.);
#5193=ORIENTED_EDGE('',*,*,#3981,.F.);
#5194=ORIENTED_EDGE('',*,*,#3986,.T.);
#5195=ORIENTED_EDGE('',*,*,#3987,.T.);
#5196=ORIENTED_EDGE('',*,*,#3988,.T.);
#5197=ORIENTED_EDGE('',*,*,#3984,.F.);
#5198=ORIENTED_EDGE('',*,*,#3989,.T.);
#5199=ORIENTED_EDGE('',*,*,#3990,.T.);
#5200=ORIENTED_EDGE('',*,*,#3991,.T.);
#5201=ORIENTED_EDGE('',*,*,#3987,.F.);
#5202=ORIENTED_EDGE('',*,*,#3992,.T.);
#5203=ORIENTED_EDGE('',*,*,#3979,.T.);
#5204=ORIENTED_EDGE('',*,*,#3993,.T.);
#5205=ORIENTED_EDGE('',*,*,#3990,.F.);
#5206=ORIENTED_EDGE('',*,*,#3992,.F.);
#5207=ORIENTED_EDGE('',*,*,#3989,.F.);
#5208=ORIENTED_EDGE('',*,*,#3986,.F.);
#5209=ORIENTED_EDGE('',*,*,#3983,.F.);
#5210=ORIENTED_EDGE('',*,*,#3980,.F.);
#5211=ORIENTED_EDGE('',*,*,#3976,.F.);
#5212=ORIENTED_EDGE('',*,*,#3993,.F.);
#5213=ORIENTED_EDGE('',*,*,#3978,.F.);
#5214=ORIENTED_EDGE('',*,*,#3982,.F.);
#5215=ORIENTED_EDGE('',*,*,#3985,.F.);
#5216=ORIENTED_EDGE('',*,*,#3988,.F.);
#5217=ORIENTED_EDGE('',*,*,#3991,.F.);
#5218=ORIENTED_EDGE('',*,*,#3994,.F.);
#5219=ORIENTED_EDGE('',*,*,#3995,.F.);
#5220=ORIENTED_EDGE('',*,*,#3996,.F.);
#5221=ORIENTED_EDGE('',*,*,#3997,.T.);
#5222=ORIENTED_EDGE('',*,*,#3995,.T.);
#5223=ORIENTED_EDGE('',*,*,#3997,.F.);
#5224=ORIENTED_EDGE('',*,*,#3998,.F.);
#5225=ORIENTED_EDGE('',*,*,#3999,.T.);
#5226=ORIENTED_EDGE('',*,*,#3996,.T.);
#5227=ORIENTED_EDGE('',*,*,#3999,.F.);
#5228=ORIENTED_EDGE('',*,*,#4000,.F.);
#5229=ORIENTED_EDGE('',*,*,#4001,.T.);
#5230=ORIENTED_EDGE('',*,*,#3998,.T.);
#5231=ORIENTED_EDGE('',*,*,#4001,.F.);
#5232=ORIENTED_EDGE('',*,*,#4000,.T.);
#5233=ORIENTED_EDGE('',*,*,#4002,.F.);
#5234=ORIENTED_EDGE('',*,*,#4003,.F.);
#5235=ORIENTED_EDGE('',*,*,#4004,.T.);
#5236=ORIENTED_EDGE('',*,*,#4002,.T.);
#5237=ORIENTED_EDGE('',*,*,#4004,.F.);
#5238=ORIENTED_EDGE('',*,*,#3994,.T.);
#5239=ORIENTED_EDGE('',*,*,#4005,.T.);
#5240=ORIENTED_EDGE('',*,*,#4003,.T.);
#5241=ORIENTED_EDGE('',*,*,#4005,.F.);
#5242=ORIENTED_EDGE('',*,*,#4006,.F.);
#5243=ORIENTED_EDGE('',*,*,#4007,.T.);
#5244=ORIENTED_EDGE('',*,*,#4008,.F.);
#5245=ORIENTED_EDGE('',*,*,#4007,.F.);
#5246=ORIENTED_EDGE('',*,*,#4009,.F.);
#5247=ORIENTED_EDGE('',*,*,#4010,.T.);
#5248=ORIENTED_EDGE('',*,*,#4011,.F.);
#5249=ORIENTED_EDGE('',*,*,#4010,.F.);
#5250=ORIENTED_EDGE('',*,*,#4012,.T.);
#5251=ORIENTED_EDGE('',*,*,#4012,.F.);
#5252=ORIENTED_EDGE('',*,*,#4009,.T.);
#5253=ORIENTED_EDGE('',*,*,#4008,.T.);
#5254=ORIENTED_EDGE('',*,*,#4013,.F.);
#5255=ORIENTED_EDGE('',*,*,#4014,.T.);
#5256=ORIENTED_EDGE('',*,*,#4015,.F.);
#5257=ORIENTED_EDGE('',*,*,#4014,.F.);
#5258=ORIENTED_EDGE('',*,*,#4016,.F.);
#5259=ORIENTED_EDGE('',*,*,#4017,.T.);
#5260=ORIENTED_EDGE('',*,*,#4018,.F.);
#5261=ORIENTED_EDGE('',*,*,#4017,.F.);
#5262=ORIENTED_EDGE('',*,*,#4015,.T.);
#5263=ORIENTED_EDGE('',*,*,#4006,.T.);
#5264=ORIENTED_EDGE('',*,*,#4016,.T.);
#5265=ORIENTED_EDGE('',*,*,#4011,.T.);
#5266=ORIENTED_EDGE('',*,*,#4019,.F.);
#5267=ORIENTED_EDGE('',*,*,#4020,.T.);
#5268=ORIENTED_EDGE('',*,*,#4021,.F.);
#5269=ORIENTED_EDGE('',*,*,#4020,.F.);
#5270=ORIENTED_EDGE('',*,*,#4022,.F.);
#5271=ORIENTED_EDGE('',*,*,#4023,.T.);
#5272=ORIENTED_EDGE('',*,*,#4024,.F.);
#5273=ORIENTED_EDGE('',*,*,#4023,.F.);
#5274=ORIENTED_EDGE('',*,*,#4025,.F.);
#5275=ORIENTED_EDGE('',*,*,#4026,.T.);
#5276=ORIENTED_EDGE('',*,*,#4027,.F.);
#5277=ORIENTED_EDGE('',*,*,#4026,.F.);
#5278=ORIENTED_EDGE('',*,*,#4028,.F.);
#5279=ORIENTED_EDGE('',*,*,#4029,.T.);
#5280=ORIENTED_EDGE('',*,*,#4030,.F.);
#5281=ORIENTED_EDGE('',*,*,#4029,.F.);
#5282=ORIENTED_EDGE('',*,*,#4031,.T.);
#5283=ORIENTED_EDGE('',*,*,#4032,.T.);
#5284=ORIENTED_EDGE('',*,*,#4033,.F.);
#5285=ORIENTED_EDGE('',*,*,#4034,.F.);
#5286=ORIENTED_EDGE('',*,*,#4035,.T.);
#5287=ORIENTED_EDGE('',*,*,#4034,.T.);
#5288=ORIENTED_EDGE('',*,*,#4036,.F.);
#5289=ORIENTED_EDGE('',*,*,#4037,.F.);
#5290=ORIENTED_EDGE('',*,*,#4038,.T.);
#5291=ORIENTED_EDGE('',*,*,#4037,.T.);
#5292=ORIENTED_EDGE('',*,*,#4039,.F.);
#5293=ORIENTED_EDGE('',*,*,#4040,.F.);
#5294=ORIENTED_EDGE('',*,*,#4041,.T.);
#5295=ORIENTED_EDGE('',*,*,#4040,.T.);
#5296=ORIENTED_EDGE('',*,*,#4042,.F.);
#5297=ORIENTED_EDGE('',*,*,#4043,.F.);
#5298=ORIENTED_EDGE('',*,*,#4044,.T.);
#5299=ORIENTED_EDGE('',*,*,#4043,.T.);
#5300=ORIENTED_EDGE('',*,*,#4045,.F.);
#5301=ORIENTED_EDGE('',*,*,#4046,.F.);
#5302=ORIENTED_EDGE('',*,*,#4047,.T.);
#5303=ORIENTED_EDGE('',*,*,#4046,.T.);
#5304=ORIENTED_EDGE('',*,*,#4048,.F.);
#5305=ORIENTED_EDGE('',*,*,#4049,.F.);
#5306=ORIENTED_EDGE('',*,*,#4050,.T.);
#5307=ORIENTED_EDGE('',*,*,#4049,.T.);
#5308=ORIENTED_EDGE('',*,*,#4051,.F.);
#5309=ORIENTED_EDGE('',*,*,#4052,.F.);
#5310=ORIENTED_EDGE('',*,*,#4053,.T.);
#5311=ORIENTED_EDGE('',*,*,#4052,.T.);
#5312=ORIENTED_EDGE('',*,*,#4054,.F.);
#5313=ORIENTED_EDGE('',*,*,#4032,.F.);
#5314=ORIENTED_EDGE('',*,*,#4054,.T.);
#5315=ORIENTED_EDGE('',*,*,#4051,.T.);
#5316=ORIENTED_EDGE('',*,*,#4048,.T.);
#5317=ORIENTED_EDGE('',*,*,#4045,.T.);
#5318=ORIENTED_EDGE('',*,*,#4042,.T.);
#5319=ORIENTED_EDGE('',*,*,#4039,.T.);
#5320=ORIENTED_EDGE('',*,*,#4036,.T.);
#5321=ORIENTED_EDGE('',*,*,#4033,.T.);
#5322=ORIENTED_EDGE('',*,*,#4018,.T.);
#5323=ORIENTED_EDGE('',*,*,#4021,.T.);
#5324=ORIENTED_EDGE('',*,*,#4024,.T.);
#5325=ORIENTED_EDGE('',*,*,#4027,.T.);
#5326=ORIENTED_EDGE('',*,*,#4030,.T.);
#5327=ORIENTED_EDGE('',*,*,#4053,.F.);
#5328=ORIENTED_EDGE('',*,*,#4031,.F.);
#5329=ORIENTED_EDGE('',*,*,#4035,.F.);
#5330=ORIENTED_EDGE('',*,*,#4038,.F.);
#5331=ORIENTED_EDGE('',*,*,#4041,.F.);
#5332=ORIENTED_EDGE('',*,*,#4044,.F.);
#5333=ORIENTED_EDGE('',*,*,#4047,.F.);
#5334=ORIENTED_EDGE('',*,*,#4050,.F.);
#5335=ORIENTED_EDGE('',*,*,#4013,.T.);
#5336=ORIENTED_EDGE('',*,*,#4019,.T.);
#5337=ORIENTED_EDGE('',*,*,#4022,.T.);
#5338=ORIENTED_EDGE('',*,*,#4025,.T.);
#5339=ORIENTED_EDGE('',*,*,#4028,.T.);
#5340=ORIENTED_EDGE('',*,*,#4055,.T.);
#5341=ORIENTED_EDGE('',*,*,#4056,.T.);
#5342=ORIENTED_EDGE('',*,*,#4057,.F.);
#5343=ORIENTED_EDGE('',*,*,#4056,.F.);
#5344=ORIENTED_EDGE('',*,*,#4058,.F.);
#5345=ORIENTED_EDGE('',*,*,#4057,.T.);
#5346=ORIENTED_EDGE('',*,*,#4059,.T.);
#5347=ORIENTED_EDGE('',*,*,#4059,.F.);
#5348=ORIENTED_EDGE('',*,*,#4058,.T.);
#5349=ORIENTED_EDGE('',*,*,#4060,.F.);
#5350=ORIENTED_EDGE('',*,*,#4060,.T.);
#5351=ORIENTED_EDGE('',*,*,#4055,.F.);
#5352=ORIENTED_EDGE('',*,*,#4061,.F.);
#5353=ORIENTED_EDGE('',*,*,#4062,.F.);
#5354=ORIENTED_EDGE('',*,*,#4063,.F.);
#5355=ORIENTED_EDGE('',*,*,#4064,.T.);
#5356=ORIENTED_EDGE('',*,*,#4065,.F.);
#5357=ORIENTED_EDGE('',*,*,#4064,.F.);
#5358=ORIENTED_EDGE('',*,*,#4066,.F.);
#5359=ORIENTED_EDGE('',*,*,#4067,.T.);
#5360=ORIENTED_EDGE('',*,*,#4068,.F.);
#5361=ORIENTED_EDGE('',*,*,#4069,.F.);
#5362=ORIENTED_EDGE('',*,*,#4070,.F.);
#5363=ORIENTED_EDGE('',*,*,#4067,.F.);
#5364=ORIENTED_EDGE('',*,*,#4071,.F.);
#5365=ORIENTED_EDGE('',*,*,#4072,.T.);
#5366=ORIENTED_EDGE('',*,*,#4073,.T.);
#5367=ORIENTED_EDGE('',*,*,#4072,.F.);
#5368=ORIENTED_EDGE('',*,*,#4062,.T.);
#5369=ORIENTED_EDGE('',*,*,#4061,.T.);
#5370=ORIENTED_EDGE('',*,*,#4063,.T.);
#5371=ORIENTED_EDGE('',*,*,#4069,.T.);
#5372=ORIENTED_EDGE('',*,*,#4068,.T.);
#5373=ORIENTED_EDGE('',*,*,#4070,.T.);
#5374=ORIENTED_EDGE('',*,*,#4074,.T.);
#5375=ORIENTED_EDGE('',*,*,#4075,.T.);
#5376=ORIENTED_EDGE('',*,*,#4076,.T.);
#5377=ORIENTED_EDGE('',*,*,#4077,.T.);
#5378=ORIENTED_EDGE('',*,*,#4078,.T.);
#5379=ORIENTED_EDGE('',*,*,#4079,.T.);
#5380=ORIENTED_EDGE('',*,*,#4080,.T.);
#5381=ORIENTED_EDGE('',*,*,#4081,.T.);
#5382=ORIENTED_EDGE('',*,*,#4082,.T.);
#5383=ORIENTED_EDGE('',*,*,#4083,.T.);
#5384=ORIENTED_EDGE('',*,*,#4084,.T.);
#5385=ORIENTED_EDGE('',*,*,#4085,.T.);
#5386=ORIENTED_EDGE('',*,*,#4075,.F.);
#5387=ORIENTED_EDGE('',*,*,#4074,.F.);
#5388=ORIENTED_EDGE('',*,*,#4076,.F.);
#5389=ORIENTED_EDGE('',*,*,#4086,.T.);
#5390=ORIENTED_EDGE('',*,*,#4087,.F.);
#5391=ORIENTED_EDGE('',*,*,#4086,.F.);
#5392=ORIENTED_EDGE('',*,*,#4088,.F.);
#5393=ORIENTED_EDGE('',*,*,#4089,.T.);
#5394=ORIENTED_EDGE('',*,*,#4078,.F.);
#5395=ORIENTED_EDGE('',*,*,#4077,.F.);
#5396=ORIENTED_EDGE('',*,*,#4079,.F.);
#5397=ORIENTED_EDGE('',*,*,#4089,.F.);
#5398=ORIENTED_EDGE('',*,*,#4081,.F.);
#5399=ORIENTED_EDGE('',*,*,#4080,.F.);
#5400=ORIENTED_EDGE('',*,*,#4082,.F.);
#5401=ORIENTED_EDGE('',*,*,#4090,.T.);
#5402=ORIENTED_EDGE('',*,*,#4091,.F.);
#5403=ORIENTED_EDGE('',*,*,#4090,.F.);
#5404=ORIENTED_EDGE('',*,*,#4092,.F.);
#5405=ORIENTED_EDGE('',*,*,#4093,.T.);
#5406=ORIENTED_EDGE('',*,*,#4084,.F.);
#5407=ORIENTED_EDGE('',*,*,#4083,.F.);
#5408=ORIENTED_EDGE('',*,*,#4085,.F.);
#5409=ORIENTED_EDGE('',*,*,#4093,.F.);
#5410=ORIENTED_EDGE('',*,*,#4073,.F.);
#5411=ORIENTED_EDGE('',*,*,#4094,.T.);
#5412=ORIENTED_EDGE('',*,*,#4095,.F.);
#5413=ORIENTED_EDGE('',*,*,#4071,.T.);
#5414=ORIENTED_EDGE('',*,*,#4096,.F.);
#5415=ORIENTED_EDGE('',*,*,#4097,.T.);
#5416=ORIENTED_EDGE('',*,*,#4095,.T.);
#5417=ORIENTED_EDGE('',*,*,#4097,.F.);
#5418=ORIENTED_EDGE('',*,*,#4096,.T.);
#5419=ORIENTED_EDGE('',*,*,#4098,.F.);
#5420=ORIENTED_EDGE('',*,*,#4098,.T.);
#5421=ORIENTED_EDGE('',*,*,#4099,.T.);
#5422=ORIENTED_EDGE('',*,*,#4094,.F.);
#5423=ORIENTED_EDGE('',*,*,#4099,.F.);
#5424=ORIENTED_EDGE('',*,*,#4066,.T.);
#5425=ORIENTED_EDGE('',*,*,#4065,.T.);
#5426=ORIENTED_EDGE('',*,*,#4088,.T.);
#5427=ORIENTED_EDGE('',*,*,#4087,.T.);
#5428=ORIENTED_EDGE('',*,*,#4092,.T.);
#5429=ORIENTED_EDGE('',*,*,#4091,.T.);
#5430=ORIENTED_EDGE('',*,*,#4100,.F.);
#5431=ORIENTED_EDGE('',*,*,#4101,.F.);
#5432=ORIENTED_EDGE('',*,*,#4102,.T.);
#5433=ORIENTED_EDGE('',*,*,#4100,.T.);
#5434=ORIENTED_EDGE('',*,*,#4102,.F.);
#5435=ORIENTED_EDGE('',*,*,#4103,.F.);
#5436=ORIENTED_EDGE('',*,*,#4104,.T.);
#5437=ORIENTED_EDGE('',*,*,#4101,.T.);
#5438=ORIENTED_EDGE('',*,*,#4104,.F.);
#5439=ORIENTED_EDGE('',*,*,#4105,.F.);
#5440=ORIENTED_EDGE('',*,*,#4106,.T.);
#5441=ORIENTED_EDGE('',*,*,#4103,.T.);
#5442=ORIENTED_EDGE('',*,*,#4106,.F.);
#5443=ORIENTED_EDGE('',*,*,#4105,.T.);
#5444=ORIENTED_EDGE('',*,*,#4107,.F.);
#5445=ORIENTED_EDGE('',*,*,#4108,.F.);
#5446=ORIENTED_EDGE('',*,*,#4109,.T.);
#5447=ORIENTED_EDGE('',*,*,#4107,.T.);
#5448=ORIENTED_EDGE('',*,*,#4109,.F.);
#5449=ORIENTED_EDGE('',*,*,#4110,.F.);
#5450=ORIENTED_EDGE('',*,*,#4111,.T.);
#5451=ORIENTED_EDGE('',*,*,#4108,.T.);
#5452=ORIENTED_EDGE('',*,*,#4111,.F.);
#5453=ORIENTED_EDGE('',*,*,#4112,.F.);
#5454=ORIENTED_EDGE('',*,*,#4113,.T.);
#5455=ORIENTED_EDGE('',*,*,#4110,.T.);
#5456=ORIENTED_EDGE('',*,*,#4113,.F.);
#5457=ORIENTED_EDGE('',*,*,#4112,.T.);
#5458=ORIENTED_EDGE('',*,*,#4114,.T.);
#5459=ORIENTED_EDGE('',*,*,#4115,.T.);
#5460=ORIENTED_EDGE('',*,*,#4116,.T.);
#5461=ORIENTED_EDGE('',*,*,#4117,.F.);
#5462=ORIENTED_EDGE('',*,*,#4118,.T.);
#5463=ORIENTED_EDGE('',*,*,#4119,.T.);
#5464=ORIENTED_EDGE('',*,*,#4120,.T.);
#5465=ORIENTED_EDGE('',*,*,#4115,.F.);
#5466=ORIENTED_EDGE('',*,*,#4121,.T.);
#5467=ORIENTED_EDGE('',*,*,#4122,.T.);
#5468=ORIENTED_EDGE('',*,*,#4123,.T.);
#5469=ORIENTED_EDGE('',*,*,#4119,.F.);
#5470=ORIENTED_EDGE('',*,*,#4124,.T.);
#5471=ORIENTED_EDGE('',*,*,#4125,.T.);
#5472=ORIENTED_EDGE('',*,*,#4126,.T.);
#5473=ORIENTED_EDGE('',*,*,#4122,.F.);
#5474=ORIENTED_EDGE('',*,*,#4127,.T.);
#5475=ORIENTED_EDGE('',*,*,#4128,.T.);
#5476=ORIENTED_EDGE('',*,*,#4129,.T.);
#5477=ORIENTED_EDGE('',*,*,#4125,.F.);
#5478=ORIENTED_EDGE('',*,*,#4130,.T.);
#5479=ORIENTED_EDGE('',*,*,#4117,.T.);
#5480=ORIENTED_EDGE('',*,*,#4131,.T.);
#5481=ORIENTED_EDGE('',*,*,#4128,.F.);
#5482=ORIENTED_EDGE('',*,*,#4130,.F.);
#5483=ORIENTED_EDGE('',*,*,#4127,.F.);
#5484=ORIENTED_EDGE('',*,*,#4124,.F.);
#5485=ORIENTED_EDGE('',*,*,#4121,.F.);
#5486=ORIENTED_EDGE('',*,*,#4118,.F.);
#5487=ORIENTED_EDGE('',*,*,#4114,.F.);
#5488=ORIENTED_EDGE('',*,*,#4131,.F.);
#5489=ORIENTED_EDGE('',*,*,#4116,.F.);
#5490=ORIENTED_EDGE('',*,*,#4120,.F.);
#5491=ORIENTED_EDGE('',*,*,#4123,.F.);
#5492=ORIENTED_EDGE('',*,*,#4126,.F.);
#5493=ORIENTED_EDGE('',*,*,#4129,.F.);
#5494=ORIENTED_EDGE('',*,*,#4132,.F.);
#5495=ORIENTED_EDGE('',*,*,#4133,.T.);
#5496=ORIENTED_EDGE('',*,*,#4134,.T.);
#5497=ORIENTED_EDGE('',*,*,#4133,.F.);
#5498=ORIENTED_EDGE('',*,*,#4135,.F.);
#5499=ORIENTED_EDGE('',*,*,#4136,.T.);
#5500=ORIENTED_EDGE('',*,*,#4137,.T.);
#5501=ORIENTED_EDGE('',*,*,#4136,.F.);
#5502=ORIENTED_EDGE('',*,*,#4135,.T.);
#5503=ORIENTED_EDGE('',*,*,#4132,.T.);
#5504=ORIENTED_EDGE('',*,*,#4137,.F.);
#5505=ORIENTED_EDGE('',*,*,#4134,.F.);
#5506=ORIENTED_EDGE('',*,*,#4138,.F.);
#5507=ORIENTED_EDGE('',*,*,#4139,.F.);
#5508=ORIENTED_EDGE('',*,*,#4140,.T.);
#5509=ORIENTED_EDGE('',*,*,#4141,.F.);
#5510=ORIENTED_EDGE('',*,*,#4140,.F.);
#5511=ORIENTED_EDGE('',*,*,#4142,.F.);
#5512=ORIENTED_EDGE('',*,*,#4143,.F.);
#5513=ORIENTED_EDGE('',*,*,#4144,.F.);
#5514=ORIENTED_EDGE('',*,*,#4145,.F.);
#5515=ORIENTED_EDGE('',*,*,#4146,.F.);
#5516=ORIENTED_EDGE('',*,*,#4147,.T.);
#5517=ORIENTED_EDGE('',*,*,#4148,.F.);
#5518=ORIENTED_EDGE('',*,*,#4149,.F.);
#5519=ORIENTED_EDGE('',*,*,#4150,.F.);
#5520=ORIENTED_EDGE('',*,*,#4151,.F.);
#5521=ORIENTED_EDGE('',*,*,#4152,.F.);
#5522=ORIENTED_EDGE('',*,*,#4153,.F.);
#5523=ORIENTED_EDGE('',*,*,#4147,.F.);
#5524=ORIENTED_EDGE('',*,*,#4143,.T.);
#5525=ORIENTED_EDGE('',*,*,#4154,.T.);
#5526=ORIENTED_EDGE('',*,*,#4152,.T.);
#5527=ORIENTED_EDGE('',*,*,#4155,.F.);
#5528=ORIENTED_EDGE('',*,*,#4142,.T.);
#5529=ORIENTED_EDGE('',*,*,#4156,.T.);
#5530=ORIENTED_EDGE('',*,*,#4153,.T.);
#5531=ORIENTED_EDGE('',*,*,#4154,.F.);
#5532=ORIENTED_EDGE('',*,*,#4139,.T.);
#5533=ORIENTED_EDGE('',*,*,#4157,.T.);
#5534=ORIENTED_EDGE('',*,*,#4148,.T.);
#5535=ORIENTED_EDGE('',*,*,#4156,.F.);
#5536=ORIENTED_EDGE('',*,*,#4158,.F.);
#5537=ORIENTED_EDGE('',*,*,#4159,.T.);
#5538=ORIENTED_EDGE('',*,*,#4160,.T.);
#5539=ORIENTED_EDGE('',*,*,#4159,.F.);
#5540=ORIENTED_EDGE('',*,*,#4138,.T.);
#5541=ORIENTED_EDGE('',*,*,#4161,.T.);
#5542=ORIENTED_EDGE('',*,*,#4149,.T.);
#5543=ORIENTED_EDGE('',*,*,#4157,.F.);
#5544=ORIENTED_EDGE('',*,*,#4144,.T.);
#5545=ORIENTED_EDGE('',*,*,#4155,.T.);
#5546=ORIENTED_EDGE('',*,*,#4151,.T.);
#5547=ORIENTED_EDGE('',*,*,#4162,.F.);
#5548=ORIENTED_EDGE('',*,*,#4145,.T.);
#5549=ORIENTED_EDGE('',*,*,#4162,.T.);
#5550=ORIENTED_EDGE('',*,*,#4150,.T.);
#5551=ORIENTED_EDGE('',*,*,#4161,.F.);
#5552=ORIENTED_EDGE('',*,*,#4146,.T.);
#5553=ORIENTED_EDGE('',*,*,#4158,.T.);
#5554=ORIENTED_EDGE('',*,*,#4141,.T.);
#5555=ORIENTED_EDGE('',*,*,#4160,.F.);
#5556=ORIENTED_EDGE('',*,*,#4163,.F.);
#5557=ORIENTED_EDGE('',*,*,#4164,.T.);
#5558=ORIENTED_EDGE('',*,*,#4165,.F.);
#5559=ORIENTED_EDGE('',*,*,#4166,.T.);
#5560=ORIENTED_EDGE('',*,*,#4167,.F.);
#5561=ORIENTED_EDGE('',*,*,#4166,.F.);
#5562=ORIENTED_EDGE('',*,*,#4168,.F.);
#5563=ORIENTED_EDGE('',*,*,#4169,.F.);
#5564=ORIENTED_EDGE('',*,*,#4170,.F.);
#5565=ORIENTED_EDGE('',*,*,#4169,.T.);
#5566=ORIENTED_EDGE('',*,*,#4171,.T.);
#5567=ORIENTED_EDGE('',*,*,#4172,.T.);
#5568=ORIENTED_EDGE('',*,*,#4168,.T.);
#5569=ORIENTED_EDGE('',*,*,#4165,.T.);
#5570=ORIENTED_EDGE('',*,*,#4173,.T.);
#5571=ORIENTED_EDGE('',*,*,#4171,.F.);
#5572=ORIENTED_EDGE('',*,*,#4174,.F.);
#5573=ORIENTED_EDGE('',*,*,#4172,.F.);
#5574=ORIENTED_EDGE('',*,*,#4173,.F.);
#5575=ORIENTED_EDGE('',*,*,#4164,.F.);
#5576=ORIENTED_EDGE('',*,*,#4175,.T.);
#5577=ORIENTED_EDGE('',*,*,#4176,.F.);
#5578=ORIENTED_EDGE('',*,*,#4177,.F.);
#5579=ORIENTED_EDGE('',*,*,#4178,.F.);
#5580=ORIENTED_EDGE('',*,*,#4175,.F.);
#5581=ORIENTED_EDGE('',*,*,#4179,.T.);
#5582=ORIENTED_EDGE('',*,*,#4177,.T.);
#5583=ORIENTED_EDGE('',*,*,#4179,.F.);
#5584=ORIENTED_EDGE('',*,*,#4178,.T.);
#5585=ORIENTED_EDGE('',*,*,#4180,.T.);
#5586=ORIENTED_EDGE('',*,*,#4181,.T.);
#5587=ORIENTED_EDGE('',*,*,#4180,.F.);
#5588=ORIENTED_EDGE('',*,*,#4182,.F.);
#5589=ORIENTED_EDGE('',*,*,#4183,.T.);
#5590=ORIENTED_EDGE('',*,*,#4176,.T.);
#5591=ORIENTED_EDGE('',*,*,#4183,.F.);
#5592=ORIENTED_EDGE('',*,*,#4170,.T.);
#5593=ORIENTED_EDGE('',*,*,#4174,.T.);
#5594=ORIENTED_EDGE('',*,*,#4163,.T.);
#5595=ORIENTED_EDGE('',*,*,#4167,.T.);
#5596=ORIENTED_EDGE('',*,*,#4182,.T.);
#5597=ORIENTED_EDGE('',*,*,#4181,.F.);
#5598=ORIENTED_EDGE('',*,*,#4184,.F.);
#5599=ORIENTED_EDGE('',*,*,#4185,.T.);
#5600=ORIENTED_EDGE('',*,*,#4186,.T.);
#5601=ORIENTED_EDGE('',*,*,#4185,.F.);
#5602=ORIENTED_EDGE('',*,*,#4187,.F.);
#5603=ORIENTED_EDGE('',*,*,#4188,.T.);
#5604=ORIENTED_EDGE('',*,*,#4189,.T.);
#5605=ORIENTED_EDGE('',*,*,#4188,.F.);
#5606=ORIENTED_EDGE('',*,*,#4187,.T.);
#5607=ORIENTED_EDGE('',*,*,#4184,.T.);
#5608=ORIENTED_EDGE('',*,*,#4189,.F.);
#5609=ORIENTED_EDGE('',*,*,#4186,.F.);
#5610=ORIENTED_EDGE('',*,*,#4190,.F.);
#5611=ORIENTED_EDGE('',*,*,#4191,.T.);
#5612=ORIENTED_EDGE('',*,*,#4192,.T.);
#5613=ORIENTED_EDGE('',*,*,#4191,.F.);
#5614=ORIENTED_EDGE('',*,*,#4193,.F.);
#5615=ORIENTED_EDGE('',*,*,#4194,.T.);
#5616=ORIENTED_EDGE('',*,*,#4195,.T.);
#5617=ORIENTED_EDGE('',*,*,#4194,.F.);
#5618=ORIENTED_EDGE('',*,*,#4193,.T.);
#5619=ORIENTED_EDGE('',*,*,#4190,.T.);
#5620=ORIENTED_EDGE('',*,*,#4195,.F.);
#5621=ORIENTED_EDGE('',*,*,#4192,.F.);
#5622=ORIENTED_EDGE('',*,*,#4196,.F.);
#5623=ORIENTED_EDGE('',*,*,#4197,.T.);
#5624=ORIENTED_EDGE('',*,*,#4198,.F.);
#5625=ORIENTED_EDGE('',*,*,#4197,.F.);
#5626=ORIENTED_EDGE('',*,*,#4199,.F.);
#5627=ORIENTED_EDGE('',*,*,#4200,.T.);
#5628=ORIENTED_EDGE('',*,*,#4201,.F.);
#5629=ORIENTED_EDGE('',*,*,#4202,.F.);
#5630=ORIENTED_EDGE('',*,*,#4203,.F.);
#5631=ORIENTED_EDGE('',*,*,#4202,.T.);
#5632=ORIENTED_EDGE('',*,*,#4204,.F.);
#5633=ORIENTED_EDGE('',*,*,#4205,.F.);
#5634=ORIENTED_EDGE('',*,*,#4206,.F.);
#5635=ORIENTED_EDGE('',*,*,#4205,.T.);
#5636=ORIENTED_EDGE('',*,*,#4207,.F.);
#5637=ORIENTED_EDGE('',*,*,#4208,.F.);
#5638=ORIENTED_EDGE('',*,*,#4209,.F.);
#5639=ORIENTED_EDGE('',*,*,#4208,.T.);
#5640=ORIENTED_EDGE('',*,*,#4210,.F.);
#5641=ORIENTED_EDGE('',*,*,#4211,.F.);
#5642=ORIENTED_EDGE('',*,*,#4212,.F.);
#5643=ORIENTED_EDGE('',*,*,#4211,.T.);
#5644=ORIENTED_EDGE('',*,*,#4213,.F.);
#5645=ORIENTED_EDGE('',*,*,#4214,.F.);
#5646=ORIENTED_EDGE('',*,*,#4215,.F.);
#5647=ORIENTED_EDGE('',*,*,#4214,.T.);
#5648=ORIENTED_EDGE('',*,*,#4216,.F.);
#5649=ORIENTED_EDGE('',*,*,#4200,.F.);
#5650=ORIENTED_EDGE('',*,*,#4216,.T.);
#5651=ORIENTED_EDGE('',*,*,#4213,.T.);
#5652=ORIENTED_EDGE('',*,*,#4210,.T.);
#5653=ORIENTED_EDGE('',*,*,#4207,.T.);
#5654=ORIENTED_EDGE('',*,*,#4204,.T.);
#5655=ORIENTED_EDGE('',*,*,#4201,.T.);
#5656=ORIENTED_EDGE('',*,*,#4198,.T.);
#5657=ORIENTED_EDGE('',*,*,#4215,.T.);
#5658=ORIENTED_EDGE('',*,*,#4199,.T.);
#5659=ORIENTED_EDGE('',*,*,#4203,.T.);
#5660=ORIENTED_EDGE('',*,*,#4206,.T.);
#5661=ORIENTED_EDGE('',*,*,#4209,.T.);
#5662=ORIENTED_EDGE('',*,*,#4212,.T.);
#5663=ORIENTED_EDGE('',*,*,#4196,.T.);
#5664=ORIENTED_EDGE('',*,*,#4217,.F.);
#5665=ORIENTED_EDGE('',*,*,#4218,.T.);
#5666=ORIENTED_EDGE('',*,*,#4219,.F.);
#5667=ORIENTED_EDGE('',*,*,#4218,.F.);
#5668=ORIENTED_EDGE('',*,*,#4220,.F.);
#5669=ORIENTED_EDGE('',*,*,#4221,.T.);
#5670=ORIENTED_EDGE('',*,*,#4222,.F.);
#5671=ORIENTED_EDGE('',*,*,#4223,.F.);
#5672=ORIENTED_EDGE('',*,*,#4224,.F.);
#5673=ORIENTED_EDGE('',*,*,#4223,.T.);
#5674=ORIENTED_EDGE('',*,*,#4225,.F.);
#5675=ORIENTED_EDGE('',*,*,#4226,.F.);
#5676=ORIENTED_EDGE('',*,*,#4227,.F.);
#5677=ORIENTED_EDGE('',*,*,#4226,.T.);
#5678=ORIENTED_EDGE('',*,*,#4228,.F.);
#5679=ORIENTED_EDGE('',*,*,#4229,.F.);
#5680=ORIENTED_EDGE('',*,*,#4230,.F.);
#5681=ORIENTED_EDGE('',*,*,#4229,.T.);
#5682=ORIENTED_EDGE('',*,*,#4231,.F.);
#5683=ORIENTED_EDGE('',*,*,#4232,.F.);
#5684=ORIENTED_EDGE('',*,*,#4233,.F.);
#5685=ORIENTED_EDGE('',*,*,#4232,.T.);
#5686=ORIENTED_EDGE('',*,*,#4234,.F.);
#5687=ORIENTED_EDGE('',*,*,#4235,.F.);
#5688=ORIENTED_EDGE('',*,*,#4236,.F.);
#5689=ORIENTED_EDGE('',*,*,#4235,.T.);
#5690=ORIENTED_EDGE('',*,*,#4237,.F.);
#5691=ORIENTED_EDGE('',*,*,#4221,.F.);
#5692=ORIENTED_EDGE('',*,*,#4237,.T.);
#5693=ORIENTED_EDGE('',*,*,#4234,.T.);
#5694=ORIENTED_EDGE('',*,*,#4231,.T.);
#5695=ORIENTED_EDGE('',*,*,#4228,.T.);
#5696=ORIENTED_EDGE('',*,*,#4225,.T.);
#5697=ORIENTED_EDGE('',*,*,#4222,.T.);
#5698=ORIENTED_EDGE('',*,*,#4219,.T.);
#5699=ORIENTED_EDGE('',*,*,#4236,.T.);
#5700=ORIENTED_EDGE('',*,*,#4220,.T.);
#5701=ORIENTED_EDGE('',*,*,#4224,.T.);
#5702=ORIENTED_EDGE('',*,*,#4227,.T.);
#5703=ORIENTED_EDGE('',*,*,#4230,.T.);
#5704=ORIENTED_EDGE('',*,*,#4233,.T.);
#5705=ORIENTED_EDGE('',*,*,#4217,.T.);
#5706=ORIENTED_EDGE('',*,*,#4238,.F.);
#5707=ORIENTED_EDGE('',*,*,#4239,.T.);
#5708=ORIENTED_EDGE('',*,*,#4240,.F.);
#5709=ORIENTED_EDGE('',*,*,#4241,.F.);
#5710=ORIENTED_EDGE('',*,*,#4242,.T.);
#5711=ORIENTED_EDGE('',*,*,#4243,.F.);
#5712=ORIENTED_EDGE('',*,*,#4244,.F.);
#5713=ORIENTED_EDGE('',*,*,#4242,.F.);
#5714=ORIENTED_EDGE('',*,*,#4245,.F.);
#5715=ORIENTED_EDGE('',*,*,#4246,.F.);
#5716=ORIENTED_EDGE('',*,*,#4239,.F.);
#5717=ORIENTED_EDGE('',*,*,#4247,.F.);
#5718=ORIENTED_EDGE('',*,*,#4245,.T.);
#5719=ORIENTED_EDGE('',*,*,#4241,.T.);
#5720=ORIENTED_EDGE('',*,*,#4248,.F.);
#5721=ORIENTED_EDGE('',*,*,#4249,.T.);
#5722=ORIENTED_EDGE('',*,*,#4250,.F.);
#5723=ORIENTED_EDGE('',*,*,#4251,.F.);
#5724=ORIENTED_EDGE('',*,*,#4252,.F.);
#5725=ORIENTED_EDGE('',*,*,#4253,.T.);
#5726=ORIENTED_EDGE('',*,*,#4254,.F.);
#5727=ORIENTED_EDGE('',*,*,#4249,.F.);
#5728=ORIENTED_EDGE('',*,*,#4255,.F.);
#5729=ORIENTED_EDGE('',*,*,#4256,.F.);
#5730=ORIENTED_EDGE('',*,*,#4257,.F.);
#5731=ORIENTED_EDGE('',*,*,#4253,.F.);
#5732=ORIENTED_EDGE('',*,*,#4258,.T.);
#5733=ORIENTED_EDGE('',*,*,#4250,.T.);
#5734=ORIENTED_EDGE('',*,*,#4254,.T.);
#5735=ORIENTED_EDGE('',*,*,#4257,.T.);
#5736=ORIENTED_EDGE('',*,*,#4259,.T.);
#5737=ORIENTED_EDGE('',*,*,#4251,.T.);
#5738=ORIENTED_EDGE('',*,*,#4259,.F.);
#5739=ORIENTED_EDGE('',*,*,#4256,.T.);
#5740=ORIENTED_EDGE('',*,*,#4260,.T.);
#5741=ORIENTED_EDGE('',*,*,#4246,.T.);
#5742=ORIENTED_EDGE('',*,*,#4247,.T.);
#5743=ORIENTED_EDGE('',*,*,#4240,.T.);
#5744=ORIENTED_EDGE('',*,*,#4238,.T.);
#5745=ORIENTED_EDGE('',*,*,#4261,.F.);
#5746=ORIENTED_EDGE('',*,*,#4262,.T.);
#5747=ORIENTED_EDGE('',*,*,#4263,.F.);
#5748=ORIENTED_EDGE('',*,*,#4262,.F.);
#5749=ORIENTED_EDGE('',*,*,#4264,.F.);
#5750=ORIENTED_EDGE('',*,*,#4265,.T.);
#5751=ORIENTED_EDGE('',*,*,#4266,.F.);
#5752=ORIENTED_EDGE('',*,*,#4265,.F.);
#5753=ORIENTED_EDGE('',*,*,#4267,.F.);
#5754=ORIENTED_EDGE('',*,*,#4268,.T.);
#5755=ORIENTED_EDGE('',*,*,#4269,.F.);
#5756=ORIENTED_EDGE('',*,*,#4268,.F.);
#5757=ORIENTED_EDGE('',*,*,#4270,.F.);
#5758=ORIENTED_EDGE('',*,*,#4271,.T.);
#5759=ORIENTED_EDGE('',*,*,#4272,.F.);
#5760=ORIENTED_EDGE('',*,*,#4271,.F.);
#5761=ORIENTED_EDGE('',*,*,#4273,.T.);
#5762=ORIENTED_EDGE('',*,*,#4274,.F.);
#5763=ORIENTED_EDGE('',*,*,#4272,.T.);
#5764=ORIENTED_EDGE('',*,*,#4269,.T.);
#5765=ORIENTED_EDGE('',*,*,#4266,.T.);
#5766=ORIENTED_EDGE('',*,*,#4263,.T.);
#5767=ORIENTED_EDGE('',*,*,#4275,.F.);
#5768=ORIENTED_EDGE('',*,*,#4276,.F.);
#5769=ORIENTED_EDGE('',*,*,#4270,.T.);
#5770=ORIENTED_EDGE('',*,*,#4267,.T.);
#5771=ORIENTED_EDGE('',*,*,#4264,.T.);
#5772=ORIENTED_EDGE('',*,*,#4261,.T.);
#5773=ORIENTED_EDGE('',*,*,#4273,.F.);
#5774=ORIENTED_EDGE('',*,*,#4277,.T.);
#5775=ORIENTED_EDGE('',*,*,#4275,.T.);
#5776=ORIENTED_EDGE('',*,*,#4277,.F.);
#5777=ORIENTED_EDGE('',*,*,#4276,.T.);
#5778=ORIENTED_EDGE('',*,*,#4278,.T.);
#5779=ORIENTED_EDGE('',*,*,#4279,.T.);
#5780=ORIENTED_EDGE('',*,*,#4278,.F.);
#5781=ORIENTED_EDGE('',*,*,#4243,.T.);
#5782=ORIENTED_EDGE('',*,*,#4244,.T.);
#5783=ORIENTED_EDGE('',*,*,#4258,.F.);
#5784=ORIENTED_EDGE('',*,*,#4280,.T.);
#5785=ORIENTED_EDGE('',*,*,#4274,.T.);
#5786=ORIENTED_EDGE('',*,*,#4280,.F.);
#5787=ORIENTED_EDGE('',*,*,#4279,.F.);
#5788=ORIENTED_EDGE('',*,*,#4248,.T.);
#5789=ORIENTED_EDGE('',*,*,#4260,.F.);
#5790=ORIENTED_EDGE('',*,*,#4255,.T.);
#5791=ORIENTED_EDGE('',*,*,#4252,.T.);
#5792=ORIENTED_EDGE('',*,*,#4281,.F.);
#5793=ORIENTED_EDGE('',*,*,#4282,.F.);
#5794=ORIENTED_EDGE('',*,*,#4283,.F.);
#5795=ORIENTED_EDGE('',*,*,#4284,.F.);
#5796=ORIENTED_EDGE('',*,*,#4285,.F.);
#5797=ORIENTED_EDGE('',*,*,#4286,.F.);
#5798=ORIENTED_EDGE('',*,*,#4287,.F.);
#5799=ORIENTED_EDGE('',*,*,#4288,.F.);
#5800=ORIENTED_EDGE('',*,*,#4285,.T.);
#5801=ORIENTED_EDGE('',*,*,#4289,.T.);
#5802=ORIENTED_EDGE('',*,*,#4290,.T.);
#5803=ORIENTED_EDGE('',*,*,#4291,.T.);
#5804=ORIENTED_EDGE('',*,*,#4284,.T.);
#5805=ORIENTED_EDGE('',*,*,#4292,.F.);
#5806=ORIENTED_EDGE('',*,*,#4293,.T.);
#5807=ORIENTED_EDGE('',*,*,#4289,.F.);
#5808=ORIENTED_EDGE('',*,*,#4283,.T.);
#5809=ORIENTED_EDGE('',*,*,#4294,.T.);
#5810=ORIENTED_EDGE('',*,*,#4295,.T.);
#5811=ORIENTED_EDGE('',*,*,#4292,.T.);
#5812=ORIENTED_EDGE('',*,*,#4282,.T.);
#5813=ORIENTED_EDGE('',*,*,#4296,.F.);
#5814=ORIENTED_EDGE('',*,*,#4297,.T.);
#5815=ORIENTED_EDGE('',*,*,#4294,.F.);
#5816=ORIENTED_EDGE('',*,*,#4290,.F.);
#5817=ORIENTED_EDGE('',*,*,#4293,.F.);
#5818=ORIENTED_EDGE('',*,*,#4295,.F.);
#5819=ORIENTED_EDGE('',*,*,#4297,.F.);
#5820=ORIENTED_EDGE('',*,*,#4298,.F.);
#5821=ORIENTED_EDGE('',*,*,#4299,.F.);
#5822=ORIENTED_EDGE('',*,*,#4300,.F.);
#5823=ORIENTED_EDGE('',*,*,#4301,.F.);
#5824=ORIENTED_EDGE('',*,*,#4281,.T.);
#5825=ORIENTED_EDGE('',*,*,#4302,.T.);
#5826=ORIENTED_EDGE('',*,*,#4298,.T.);
#5827=ORIENTED_EDGE('',*,*,#4296,.T.);
#5828=ORIENTED_EDGE('',*,*,#4288,.T.);
#5829=ORIENTED_EDGE('',*,*,#4303,.F.);
#5830=ORIENTED_EDGE('',*,*,#4299,.T.);
#5831=ORIENTED_EDGE('',*,*,#4302,.F.);
#5832=ORIENTED_EDGE('',*,*,#4287,.T.);
#5833=ORIENTED_EDGE('',*,*,#4304,.T.);
#5834=ORIENTED_EDGE('',*,*,#4300,.T.);
#5835=ORIENTED_EDGE('',*,*,#4303,.T.);
#5836=ORIENTED_EDGE('',*,*,#4286,.T.);
#5837=ORIENTED_EDGE('',*,*,#4291,.F.);
#5838=ORIENTED_EDGE('',*,*,#4301,.T.);
#5839=ORIENTED_EDGE('',*,*,#4304,.F.);
#5840=ORIENTED_EDGE('',*,*,#4305,.F.);
#5841=ORIENTED_EDGE('',*,*,#4306,.T.);
#5842=ORIENTED_EDGE('',*,*,#4307,.T.);
#5843=ORIENTED_EDGE('',*,*,#4308,.F.);
#5844=ORIENTED_EDGE('',*,*,#4309,.F.);
#5845=ORIENTED_EDGE('',*,*,#4310,.T.);
#5846=ORIENTED_EDGE('',*,*,#4311,.T.);
#5847=ORIENTED_EDGE('',*,*,#4306,.F.);
#5848=ORIENTED_EDGE('',*,*,#4312,.F.);
#5849=ORIENTED_EDGE('',*,*,#4313,.T.);
#5850=ORIENTED_EDGE('',*,*,#4314,.T.);
#5851=ORIENTED_EDGE('',*,*,#4310,.F.);
#5852=ORIENTED_EDGE('',*,*,#4315,.F.);
#5853=ORIENTED_EDGE('',*,*,#4316,.T.);
#5854=ORIENTED_EDGE('',*,*,#4317,.T.);
#5855=ORIENTED_EDGE('',*,*,#4313,.F.);
#5856=ORIENTED_EDGE('',*,*,#4318,.F.);
#5857=ORIENTED_EDGE('',*,*,#4319,.T.);
#5858=ORIENTED_EDGE('',*,*,#4320,.T.);
#5859=ORIENTED_EDGE('',*,*,#4316,.F.);
#5860=ORIENTED_EDGE('',*,*,#4321,.F.);
#5861=ORIENTED_EDGE('',*,*,#4308,.T.);
#5862=ORIENTED_EDGE('',*,*,#4322,.T.);
#5863=ORIENTED_EDGE('',*,*,#4319,.F.);
#5864=ORIENTED_EDGE('',*,*,#4322,.F.);
#5865=ORIENTED_EDGE('',*,*,#4307,.F.);
#5866=ORIENTED_EDGE('',*,*,#4311,.F.);
#5867=ORIENTED_EDGE('',*,*,#4314,.F.);
#5868=ORIENTED_EDGE('',*,*,#4317,.F.);
#5869=ORIENTED_EDGE('',*,*,#4320,.F.);
#5870=ORIENTED_EDGE('',*,*,#4323,.F.);
#5871=ORIENTED_EDGE('',*,*,#4305,.T.);
#5872=ORIENTED_EDGE('',*,*,#4321,.T.);
#5873=ORIENTED_EDGE('',*,*,#4318,.T.);
#5874=ORIENTED_EDGE('',*,*,#4315,.T.);
#5875=ORIENTED_EDGE('',*,*,#4312,.T.);
#5876=ORIENTED_EDGE('',*,*,#4309,.T.);
#5877=ORIENTED_EDGE('',*,*,#4324,.F.);
#5878=ORIENTED_EDGE('',*,*,#4325,.T.);
#5879=ORIENTED_EDGE('',*,*,#4323,.T.);
#5880=ORIENTED_EDGE('',*,*,#4325,.F.);
#5881=ORIENTED_EDGE('',*,*,#4326,.F.);
#5882=ORIENTED_EDGE('',*,*,#4327,.T.);
#5883=ORIENTED_EDGE('',*,*,#4324,.T.);
#5884=ORIENTED_EDGE('',*,*,#4327,.F.);
#5885=ORIENTED_EDGE('',*,*,#4328,.F.);
#5886=ORIENTED_EDGE('',*,*,#4329,.T.);
#5887=ORIENTED_EDGE('',*,*,#4326,.T.);
#5888=ORIENTED_EDGE('',*,*,#4329,.F.);
#5889=ORIENTED_EDGE('',*,*,#4328,.T.);
#5890=CYLINDRICAL_SURFACE('',#6716,0.25);
#5891=CYLINDRICAL_SURFACE('',#6719,0.25);
#5892=CYLINDRICAL_SURFACE('',#6722,0.25);
#5893=CYLINDRICAL_SURFACE('',#6725,0.25);
#5894=CYLINDRICAL_SURFACE('',#6728,0.275);
#5895=CYLINDRICAL_SURFACE('',#6731,0.275);
#5896=CYLINDRICAL_SURFACE('',#6734,0.275);
#5897=CYLINDRICAL_SURFACE('',#6737,0.275);
#5898=CYLINDRICAL_SURFACE('',#6740,0.275);
#5899=CYLINDRICAL_SURFACE('',#6743,0.275);
#5900=CYLINDRICAL_SURFACE('',#6746,0.275);
#5901=CYLINDRICAL_SURFACE('',#6749,0.275);
#5902=CYLINDRICAL_SURFACE('',#6787,0.33);
#5903=CYLINDRICAL_SURFACE('',#6790,0.33);
#5904=CYLINDRICAL_SURFACE('',#6793,0.44);
#5905=CYLINDRICAL_SURFACE('',#6796,0.44);
#5906=CYLINDRICAL_SURFACE('',#6799,0.44);
#5907=CYLINDRICAL_SURFACE('',#6802,0.44);
#5908=CYLINDRICAL_SURFACE('',#6805,3.1);
#5909=CYLINDRICAL_SURFACE('',#6817,0.425);
#5910=CYLINDRICAL_SURFACE('',#6820,0.595);
#5911=CYLINDRICAL_SURFACE('',#6826,0.425);
#5912=CYLINDRICAL_SURFACE('',#6829,0.595);
#5913=CYLINDRICAL_SURFACE('',#6835,0.425);
#5914=CYLINDRICAL_SURFACE('',#6838,0.595);
#5915=CYLINDRICAL_SURFACE('',#6844,0.425);
#5916=CYLINDRICAL_SURFACE('',#6847,0.595);
#5917=CYLINDRICAL_SURFACE('',#6853,0.33);
#5918=CYLINDRICAL_SURFACE('',#6856,0.33);
#5919=CYLINDRICAL_SURFACE('',#6859,0.44);
#5920=CYLINDRICAL_SURFACE('',#6862,0.44);
#5921=CYLINDRICAL_SURFACE('',#6865,0.44);
#5922=CYLINDRICAL_SURFACE('',#6868,0.44);
#5923=CYLINDRICAL_SURFACE('',#6871,3.1);
#5924=CYLINDRICAL_SURFACE('',#6883,0.425);
#5925=CYLINDRICAL_SURFACE('',#6886,0.595);
#5926=CYLINDRICAL_SURFACE('',#6892,0.425);
#5927=CYLINDRICAL_SURFACE('',#6895,0.595);
#5928=CYLINDRICAL_SURFACE('',#6901,0.425);
#5929=CYLINDRICAL_SURFACE('',#6904,0.595);
#5930=CYLINDRICAL_SURFACE('',#6910,0.425);
#5931=CYLINDRICAL_SURFACE('',#6913,0.595);
#5932=CYLINDRICAL_SURFACE('',#6955,0.21);
#5933=CYLINDRICAL_SURFACE('',#6980,0.2117);
#5934=CYLINDRICAL_SURFACE('',#7004,0.425);
#5935=CYLINDRICAL_SURFACE('',#7012,0.24505);
#5936=CYLINDRICAL_SURFACE('',#7028,0.5);
#5937=CYLINDRICAL_SURFACE('',#7036,0.2942);
#5938=CYLINDRICAL_SURFACE('',#7039,2.05);
#5939=CYLINDRICAL_SURFACE('',#7042,2.05);
#5940=CYLINDRICAL_SURFACE('',#7047,3.);
#5941=CYLINDRICAL_SURFACE('',#7050,3.);
#5942=CYLINDRICAL_SURFACE('',#7055,0.6);
#5943=CYLINDRICAL_SURFACE('',#7058,0.6);
#5944=CYLINDRICAL_SURFACE('',#7061,0.6);
#5945=CYLINDRICAL_SURFACE('',#7064,0.6);
#5946=CYLINDRICAL_SURFACE('',#7078,1.8);
#5947=CYLINDRICAL_SURFACE('',#7087,0.25);
#5948=CYLINDRICAL_SURFACE('',#7088,0.25);
#5949=CYLINDRICAL_SURFACE('',#7089,1.65);
#5950=CYLINDRICAL_SURFACE('',#7092,0.25);
#5951=CYLINDRICAL_SURFACE('',#7093,0.25);
#5952=CYLINDRICAL_SURFACE('',#7094,0.25);
#5953=CYLINDRICAL_SURFACE('',#7095,0.25);
#5954=CYLINDRICAL_SURFACE('',#7100,1.75);
#5955=CYLINDRICAL_SURFACE('',#7104,0.6);
#5956=CYLINDRICAL_SURFACE('',#7112,0.65);
#5957=CYLINDRICAL_SURFACE('',#7120,0.3933);
#5958=CYLINDRICAL_SURFACE('',#7134,0.42);
#5959=CYLINDRICAL_SURFACE('',#7137,0.8);
#5960=CYLINDRICAL_SURFACE('',#7150,0.338975);
#5961=CYLINDRICAL_SURFACE('',#7246,1.);
#5962=CYLINDRICAL_SURFACE('',#7247,0.6);
#5963=CYLINDRICAL_SURFACE('',#7249,0.6);
#5964=CYLINDRICAL_SURFACE('',#7254,0.605);
#5965=CYLINDRICAL_SURFACE('',#7257,1.);
#5966=CYLINDRICAL_SURFACE('',#7263,0.605);
#5967=CYLINDRICAL_SURFACE('',#7266,1.);
#5968=CYLINDRICAL_SURFACE('',#7272,0.54);
#5969=CYLINDRICAL_SURFACE('',#7284,0.54);
#5970=CYLINDRICAL_SURFACE('',#7298,0.21);
#5971=CYLINDRICAL_SURFACE('',#7308,0.6);
#5972=CYLINDRICAL_SURFACE('',#7310,0.275);
#5973=CYLINDRICAL_SURFACE('',#7313,0.275);
#5974=CYLINDRICAL_SURFACE('',#7316,0.275);
#5975=CYLINDRICAL_SURFACE('',#7319,0.275);
#5976=CYLINDRICAL_SURFACE('',#7328,3.);
#5977=CYLINDRICAL_SURFACE('',#7329,1.5);
#5978=CYLINDRICAL_SURFACE('',#7331,1.5);
#5979=CYLINDRICAL_SURFACE('',#7356,0.24505);
#5980=ADVANCED_FACE('',(#917),#5890,.F.);
#5981=ADVANCED_FACE('',(#918),#5891,.F.);
#5982=ADVANCED_FACE('',(#919),#5892,.F.);
#5983=ADVANCED_FACE('',(#920),#5893,.F.);
#5984=ADVANCED_FACE('',(#921),#5894,.F.);
#5985=ADVANCED_FACE('',(#922),#5895,.F.);
#5986=ADVANCED_FACE('',(#923),#5896,.F.);
#5987=ADVANCED_FACE('',(#924),#5897,.F.);
#5988=ADVANCED_FACE('',(#925),#5898,.F.);
#5989=ADVANCED_FACE('',(#926),#5899,.F.);
#5990=ADVANCED_FACE('',(#927),#5900,.F.);
#5991=ADVANCED_FACE('',(#928),#5901,.F.);
#5992=ADVANCED_FACE('',(#929),#679,.T.);
#5993=ADVANCED_FACE('',(#930),#680,.T.);
#5994=ADVANCED_FACE('',(#931),#681,.T.);
#5995=ADVANCED_FACE('',(#932),#682,.T.);
#5996=ADVANCED_FACE('',(#933,#542,#543,#544,#545,#546,#547,#548,#549,#550,
#551,#552,#553),#683,.T.);
#5997=ADVANCED_FACE('',(#934,#554,#555,#556,#557,#558,#559,#560,#561,#562,
#563,#564,#565),#684,.F.);
#5998=ADVANCED_FACE('',(#935),#685,.T.);
#5999=ADVANCED_FACE('',(#936),#686,.T.);
#6000=ADVANCED_FACE('',(#937),#687,.T.);
#6001=ADVANCED_FACE('',(#938),#688,.T.);
#6002=ADVANCED_FACE('',(#939),#689,.T.);
#6003=ADVANCED_FACE('',(#940),#690,.F.);
#6004=ADVANCED_FACE('',(#941),#691,.T.);
#6005=ADVANCED_FACE('',(#942),#692,.T.);
#6006=ADVANCED_FACE('',(#943),#693,.T.);
#6007=ADVANCED_FACE('',(#944),#694,.T.);
#6008=ADVANCED_FACE('',(#945),#695,.T.);
#6009=ADVANCED_FACE('',(#946),#696,.F.);
#6010=ADVANCED_FACE('',(#947),#697,.T.);
#6011=ADVANCED_FACE('',(#948),#698,.T.);
#6012=ADVANCED_FACE('',(#949),#699,.T.);
#6013=ADVANCED_FACE('',(#950),#700,.T.);
#6014=ADVANCED_FACE('',(#951),#701,.T.);
#6015=ADVANCED_FACE('',(#952),#702,.F.);
#6016=ADVANCED_FACE('',(#953),#703,.T.);
#6017=ADVANCED_FACE('',(#954),#704,.T.);
#6018=ADVANCED_FACE('',(#955),#705,.T.);
#6019=ADVANCED_FACE('',(#956),#706,.T.);
#6020=ADVANCED_FACE('',(#957),#707,.T.);
#6021=ADVANCED_FACE('',(#958),#708,.F.);
#6022=ADVANCED_FACE('',(#959),#5902,.F.);
#6023=ADVANCED_FACE('',(#960),#5903,.F.);
#6024=ADVANCED_FACE('',(#961),#5904,.F.);
#6025=ADVANCED_FACE('',(#962),#5905,.F.);
#6026=ADVANCED_FACE('',(#963),#5906,.F.);
#6027=ADVANCED_FACE('',(#964),#5907,.F.);
#6028=ADVANCED_FACE('',(#965),#5908,.F.);
#6029=ADVANCED_FACE('',(#966,#566,#567),#709,.T.);
#6030=ADVANCED_FACE('',(#967),#710,.F.);
#6031=ADVANCED_FACE('',(#968,#568,#569,#570,#571,#572),#711,.T.);
#6032=ADVANCED_FACE('',(#969),#712,.T.);
#6033=ADVANCED_FACE('',(#970),#713,.T.);
#6034=ADVANCED_FACE('',(#971,#573,#574,#575,#576,#577),#714,.T.);
#6035=ADVANCED_FACE('',(#972),#715,.T.);
#6036=ADVANCED_FACE('',(#973,#578,#579),#716,.F.);
#6037=ADVANCED_FACE('',(#974),#5909,.F.);
#6038=ADVANCED_FACE('',(#975),#5910,.T.);
#6039=ADVANCED_FACE('',(#976,#580),#717,.T.);
#6040=ADVANCED_FACE('',(#977,#581),#718,.F.);
#6041=ADVANCED_FACE('',(#978),#5911,.F.);
#6042=ADVANCED_FACE('',(#979),#5912,.T.);
#6043=ADVANCED_FACE('',(#980,#582),#719,.T.);
#6044=ADVANCED_FACE('',(#981,#583),#720,.F.);
#6045=ADVANCED_FACE('',(#982),#5913,.F.);
#6046=ADVANCED_FACE('',(#983),#5914,.T.);
#6047=ADVANCED_FACE('',(#984,#584),#721,.T.);
#6048=ADVANCED_FACE('',(#985,#585),#722,.F.);
#6049=ADVANCED_FACE('',(#986),#5915,.F.);
#6050=ADVANCED_FACE('',(#987),#5916,.T.);
#6051=ADVANCED_FACE('',(#988,#586),#723,.T.);
#6052=ADVANCED_FACE('',(#989,#587),#724,.F.);
#6053=ADVANCED_FACE('',(#990),#5917,.F.);
#6054=ADVANCED_FACE('',(#991),#5918,.F.);
#6055=ADVANCED_FACE('',(#992),#5919,.F.);
#6056=ADVANCED_FACE('',(#993),#5920,.F.);
#6057=ADVANCED_FACE('',(#994),#5921,.F.);
#6058=ADVANCED_FACE('',(#995),#5922,.F.);
#6059=ADVANCED_FACE('',(#996),#5923,.F.);
#6060=ADVANCED_FACE('',(#997,#588,#589),#725,.T.);
#6061=ADVANCED_FACE('',(#998),#726,.F.);
#6062=ADVANCED_FACE('',(#999,#590,#591,#592,#593,#594),#727,.T.);
#6063=ADVANCED_FACE('',(#1000),#728,.T.);
#6064=ADVANCED_FACE('',(#1001),#729,.T.);
#6065=ADVANCED_FACE('',(#1002,#595,#596,#597,#598,#599),#730,.T.);
#6066=ADVANCED_FACE('',(#1003),#731,.T.);
#6067=ADVANCED_FACE('',(#1004,#600,#601),#732,.F.);
#6068=ADVANCED_FACE('',(#1005),#5924,.F.);
#6069=ADVANCED_FACE('',(#1006),#5925,.T.);
#6070=ADVANCED_FACE('',(#1007,#602),#733,.T.);
#6071=ADVANCED_FACE('',(#1008,#603),#734,.F.);
#6072=ADVANCED_FACE('',(#1009),#5926,.F.);
#6073=ADVANCED_FACE('',(#1010),#5927,.T.);
#6074=ADVANCED_FACE('',(#1011,#604),#735,.T.);
#6075=ADVANCED_FACE('',(#1012,#605),#736,.F.);
#6076=ADVANCED_FACE('',(#1013),#5928,.F.);
#6077=ADVANCED_FACE('',(#1014),#5929,.T.);
#6078=ADVANCED_FACE('',(#1015,#606),#737,.T.);
#6079=ADVANCED_FACE('',(#1016,#607),#738,.F.);
#6080=ADVANCED_FACE('',(#1017),#5930,.F.);
#6081=ADVANCED_FACE('',(#1018),#5931,.T.);
#6082=ADVANCED_FACE('',(#1019,#608),#739,.T.);
#6083=ADVANCED_FACE('',(#1020,#609),#740,.F.);
#6084=ADVANCED_FACE('',(#1021),#741,.F.);
#6085=ADVANCED_FACE('',(#1022),#742,.F.);
#6086=ADVANCED_FACE('',(#1023),#743,.F.);
#6087=ADVANCED_FACE('',(#1024),#744,.F.);
#6088=ADVANCED_FACE('',(#1025),#745,.F.);
#6089=ADVANCED_FACE('',(#1026),#746,.F.);
#6090=ADVANCED_FACE('',(#1027),#747,.F.);
#6091=ADVANCED_FACE('',(#1028),#748,.F.);
#6092=ADVANCED_FACE('',(#1029),#749,.F.);
#6093=ADVANCED_FACE('',(#1030),#750,.F.);
#6094=ADVANCED_FACE('',(#1031),#751,.F.);
#6095=ADVANCED_FACE('',(#1032),#752,.F.);
#6096=ADVANCED_FACE('',(#1033),#753,.F.);
#6097=ADVANCED_FACE('',(#1034),#754,.F.);
#6098=ADVANCED_FACE('',(#1035),#755,.F.);
#6099=ADVANCED_FACE('',(#1036),#756,.F.);
#6100=ADVANCED_FACE('',(#1037),#757,.F.);
#6101=ADVANCED_FACE('',(#1038),#758,.F.);
#6102=ADVANCED_FACE('',(#1039),#759,.F.);
#6103=ADVANCED_FACE('',(#1040),#760,.F.);
#6104=ADVANCED_FACE('',(#1041),#761,.F.);
#6105=ADVANCED_FACE('',(#1042),#762,.F.);
#6106=ADVANCED_FACE('',(#1043),#763,.F.);
#6107=ADVANCED_FACE('',(#1044),#764,.F.);
#6108=ADVANCED_FACE('',(#1045),#765,.F.);
#6109=ADVANCED_FACE('',(#1046),#766,.F.);
#6110=ADVANCED_FACE('',(#1047),#767,.F.);
#6111=ADVANCED_FACE('',(#1048),#768,.F.);
#6112=ADVANCED_FACE('',(#1049),#769,.F.);
#6113=ADVANCED_FACE('',(#1050),#770,.F.);
#6114=ADVANCED_FACE('',(#1051),#771,.F.);
#6115=ADVANCED_FACE('',(#1052),#772,.F.);
#6116=ADVANCED_FACE('',(#1053),#773,.F.);
#6117=ADVANCED_FACE('',(#1054),#774,.F.);
#6118=ADVANCED_FACE('',(#1055),#775,.F.);
#6119=ADVANCED_FACE('',(#1056),#776,.F.);
#6120=ADVANCED_FACE('',(#1057),#5932,.F.);
#6121=ADVANCED_FACE('',(#1058),#777,.T.);
#6122=ADVANCED_FACE('',(#1059),#778,.T.);
#6123=ADVANCED_FACE('',(#1060),#779,.T.);
#6124=ADVANCED_FACE('',(#1061),#780,.T.);
#6125=ADVANCED_FACE('',(#1062),#781,.T.);
#6126=ADVANCED_FACE('',(#1063),#782,.T.);
#6127=ADVANCED_FACE('',(#1064),#783,.T.);
#6128=ADVANCED_FACE('',(#1065),#784,.T.);
#6129=ADVANCED_FACE('',(#1066,#610),#785,.T.);
#6130=ADVANCED_FACE('',(#1067,#611),#786,.F.);
#6131=ADVANCED_FACE('',(#1068),#787,.F.);
#6132=ADVANCED_FACE('',(#1069),#788,.T.);
#6133=ADVANCED_FACE('',(#1070,#612),#789,.T.);
#6134=ADVANCED_FACE('',(#1071),#790,.T.);
#6135=ADVANCED_FACE('',(#1072),#791,.T.);
#6136=ADVANCED_FACE('',(#1073),#792,.F.);
#6137=ADVANCED_FACE('',(#1074),#793,.T.);
#6138=ADVANCED_FACE('',(#1075),#794,.T.);
#6139=ADVANCED_FACE('',(#1076),#795,.T.);
#6140=ADVANCED_FACE('',(#1077),#5933,.F.);
#6141=ADVANCED_FACE('',(#1078),#796,.F.);
#6142=ADVANCED_FACE('',(#1079),#797,.F.);
#6143=ADVANCED_FACE('',(#1080),#798,.T.);
#6144=ADVANCED_FACE('',(#1081),#799,.T.);
#6145=ADVANCED_FACE('',(#1082),#800,.F.);
#6146=ADVANCED_FACE('',(#1083),#801,.F.);
#6147=ADVANCED_FACE('',(#1084),#802,.F.);
#6148=ADVANCED_FACE('',(#1085),#803,.F.);
#6149=ADVANCED_FACE('',(#1086),#804,.F.);
#6150=ADVANCED_FACE('',(#1087),#805,.F.);
#6151=ADVANCED_FACE('',(#1088),#806,.F.);
#6152=ADVANCED_FACE('',(#1089),#807,.F.);
#6153=ADVANCED_FACE('',(#1090),#808,.F.);
#6154=ADVANCED_FACE('',(#1091),#809,.T.);
#6155=ADVANCED_FACE('',(#1092),#393,.T.);
#6156=ADVANCED_FACE('',(#1093),#5934,.T.);
#6157=ADVANCED_FACE('',(#1094),#394,.T.);
#6158=ADVANCED_FACE('',(#1095,#613),#810,.T.);
#6159=ADVANCED_FACE('',(#1096),#395,.T.);
#6160=ADVANCED_FACE('',(#1097),#5935,.T.);
#6161=ADVANCED_FACE('',(#1098),#811,.F.);
#6162=ADVANCED_FACE('',(#1099),#812,.F.);
#6163=ADVANCED_FACE('',(#1100),#813,.F.);
#6164=ADVANCED_FACE('',(#1101),#814,.F.);
#6165=ADVANCED_FACE('',(#1102),#815,.F.);
#6166=ADVANCED_FACE('',(#1103),#816,.F.);
#6167=ADVANCED_FACE('',(#1104),#817,.F.);
#6168=ADVANCED_FACE('',(#1105),#818,.F.);
#6169=ADVANCED_FACE('',(#1106),#819,.F.);
#6170=ADVANCED_FACE('',(#1107),#820,.T.);
#6171=ADVANCED_FACE('',(#1108),#396,.T.);
#6172=ADVANCED_FACE('',(#1109),#5936,.T.);
#6173=ADVANCED_FACE('',(#1110),#397,.T.);
#6174=ADVANCED_FACE('',(#1111,#614),#821,.T.);
#6175=ADVANCED_FACE('',(#1112),#398,.T.);
#6176=ADVANCED_FACE('',(#1113),#5937,.T.);
#6177=ADVANCED_FACE('',(#1114),#5938,.F.);
#6178=ADVANCED_FACE('',(#1115),#5939,.F.);
#6179=ADVANCED_FACE('',(#1116,#615,#616),#391,.F.);
#6180=ADVANCED_FACE('',(#1117),#5940,.T.);
#6181=ADVANCED_FACE('',(#1118),#5941,.T.);
#6182=ADVANCED_FACE('',(#1119,#617),#822,.F.);
#6183=ADVANCED_FACE('',(#1120,#618),#823,.T.);
#6184=ADVANCED_FACE('',(#1121),#5942,.F.);
#6185=ADVANCED_FACE('',(#1122),#5943,.F.);
#6186=ADVANCED_FACE('',(#1123),#5944,.F.);
#6187=ADVANCED_FACE('',(#1124),#5945,.F.);
#6188=ADVANCED_FACE('',(#1125),#824,.T.);
#6189=ADVANCED_FACE('',(#1126),#825,.T.);
#6190=ADVANCED_FACE('',(#1127),#826,.T.);
#6191=ADVANCED_FACE('',(#1128),#827,.T.);
#6192=ADVANCED_FACE('',(#1129),#828,.T.);
#6193=ADVANCED_FACE('',(#1130),#829,.T.);
#6194=ADVANCED_FACE('',(#1131),#830,.T.);
#6195=ADVANCED_FACE('',(#1132),#831,.T.);
#6196=ADVANCED_FACE('',(#1133,#619,#620,#621,#622,#623),#832,.T.);
#6197=ADVANCED_FACE('',(#1134,#624,#625,#626,#627,#628),#833,.F.);
#6198=ADVANCED_FACE('',(#1135),#5946,.F.);
#6199=ADVANCED_FACE('',(#1136,#629),#834,.T.);
#6200=ADVANCED_FACE('',(#1137,#630,#631),#392,.T.);
#6201=ADVANCED_FACE('',(#1138,#632),#835,.T.);
#6202=ADVANCED_FACE('',(#1139),#5947,.F.);
#6203=ADVANCED_FACE('',(#1140),#5948,.F.);
#6204=ADVANCED_FACE('',(#1141,#633,#634,#635,#636,#637,#638),#5949,.T.);
#6205=ADVANCED_FACE('',(#1142),#5950,.F.);
#6206=ADVANCED_FACE('',(#1143),#5951,.F.);
#6207=ADVANCED_FACE('',(#1144),#5952,.F.);
#6208=ADVANCED_FACE('',(#1145),#5953,.F.);
#6209=ADVANCED_FACE('',(#1146,#639),#836,.T.);
#6210=ADVANCED_FACE('',(#1147,#640),#837,.T.);
#6211=ADVANCED_FACE('',(#1148),#5954,.T.);
#6212=ADVANCED_FACE('',(#1149,#641),#838,.T.);
#6213=ADVANCED_FACE('',(#1150,#642,#643,#644,#645,#646,#647),#5955,.F.);
#6214=ADVANCED_FACE('',(#1151),#839,.T.);
#6215=ADVANCED_FACE('',(#1152),#399,.T.);
#6216=ADVANCED_FACE('',(#1153),#5956,.T.);
#6217=ADVANCED_FACE('',(#1154),#400,.T.);
#6218=ADVANCED_FACE('',(#1155,#648),#840,.T.);
#6219=ADVANCED_FACE('',(#1156),#401,.T.);
#6220=ADVANCED_FACE('',(#1157),#5957,.T.);
#6221=ADVANCED_FACE('',(#1158),#402,.T.);
#6222=ADVANCED_FACE('',(#1159),#841,.T.);
#6223=ADVANCED_FACE('',(#1160),#842,.F.);
#6224=ADVANCED_FACE('',(#1161),#843,.F.);
#6225=ADVANCED_FACE('',(#1162),#844,.F.);
#6226=ADVANCED_FACE('',(#1163),#845,.F.);
#6227=ADVANCED_FACE('',(#1164),#846,.F.);
#6228=ADVANCED_FACE('',(#1165),#847,.F.);
#6229=ADVANCED_FACE('',(#1166),#848,.F.);
#6230=ADVANCED_FACE('',(#1167),#849,.F.);
#6231=ADVANCED_FACE('',(#1168),#5958,.F.);
#6232=ADVANCED_FACE('',(#1169),#5959,.T.);
#6233=ADVANCED_FACE('',(#1170,#649),#850,.T.);
#6234=ADVANCED_FACE('',(#1171,#650),#851,.F.);
#6235=ADVANCED_FACE('',(#1172),#403,.T.);
#6236=ADVANCED_FACE('',(#1173),#404,.T.);
#6237=ADVANCED_FACE('',(#1174),#852,.T.);
#6238=ADVANCED_FACE('',(#1175),#853,.T.);
#6239=ADVANCED_FACE('',(#1176),#854,.T.);
#6240=ADVANCED_FACE('',(#1177),#5960,.F.);
#6241=ADVANCED_FACE('',(#1178),#855,.T.);
#6242=ADVANCED_FACE('',(#1179),#856,.T.);
#6243=ADVANCED_FACE('',(#1180),#857,.T.);
#6244=ADVANCED_FACE('',(#1181,#651),#858,.T.);
#6245=ADVANCED_FACE('',(#1182,#652),#859,.F.);
#6246=ADVANCED_FACE('',(#1183),#860,.F.);
#6247=ADVANCED_FACE('',(#1184),#861,.T.);
#6248=ADVANCED_FACE('',(#1185),#862,.F.);
#6249=ADVANCED_FACE('',(#1186),#863,.F.);
#6250=ADVANCED_FACE('',(#1187),#864,.F.);
#6251=ADVANCED_FACE('',(#1188,#653),#865,.T.);
#6252=ADVANCED_FACE('',(#1189,#654),#866,.F.);
#6253=ADVANCED_FACE('',(#1190),#5961,.T.);
#6254=ADVANCED_FACE('',(#1191),#5962,.T.);
#6255=ADVANCED_FACE('',(#1192,#655),#5963,.T.);
#6256=ADVANCED_FACE('',(#1193),#867,.T.);
#6257=ADVANCED_FACE('',(#1194),#868,.F.);
#6258=ADVANCED_FACE('',(#1195),#5964,.F.);
#6259=ADVANCED_FACE('',(#1196),#5965,.T.);
#6260=ADVANCED_FACE('',(#1197,#656),#869,.T.);
#6261=ADVANCED_FACE('',(#1198,#657),#870,.F.);
#6262=ADVANCED_FACE('',(#1199),#5966,.F.);
#6263=ADVANCED_FACE('',(#1200),#5967,.T.);
#6264=ADVANCED_FACE('',(#1201,#658),#871,.T.);
#6265=ADVANCED_FACE('',(#1202,#659),#872,.F.);
#6266=ADVANCED_FACE('',(#1203),#5968,.F.);
#6267=ADVANCED_FACE('',(#1204),#873,.T.);
#6268=ADVANCED_FACE('',(#1205),#874,.T.);
#6269=ADVANCED_FACE('',(#1206),#875,.T.);
#6270=ADVANCED_FACE('',(#1207),#876,.T.);
#6271=ADVANCED_FACE('',(#1208),#877,.T.);
#6272=ADVANCED_FACE('',(#1209),#878,.T.);
#6273=ADVANCED_FACE('',(#1210,#660),#879,.T.);
#6274=ADVANCED_FACE('',(#1211,#661),#880,.F.);
#6275=ADVANCED_FACE('',(#1212),#5969,.F.);
#6276=ADVANCED_FACE('',(#1213),#881,.T.);
#6277=ADVANCED_FACE('',(#1214),#882,.T.);
#6278=ADVANCED_FACE('',(#1215),#883,.T.);
#6279=ADVANCED_FACE('',(#1216),#884,.T.);
#6280=ADVANCED_FACE('',(#1217),#885,.T.);
#6281=ADVANCED_FACE('',(#1218),#886,.T.);
#6282=ADVANCED_FACE('',(#1219,#662),#887,.T.);
#6283=ADVANCED_FACE('',(#1220,#663),#888,.F.);
#6284=ADVANCED_FACE('',(#1221),#889,.T.);
#6285=ADVANCED_FACE('',(#1222),#5970,.F.);
#6286=ADVANCED_FACE('',(#1223),#890,.T.);
#6287=ADVANCED_FACE('',(#1224),#891,.F.);
#6288=ADVANCED_FACE('',(#1225),#892,.F.);
#6289=ADVANCED_FACE('',(#1226),#893,.F.);
#6290=ADVANCED_FACE('',(#1227,#664),#894,.T.);
#6291=ADVANCED_FACE('',(#1228,#665),#5971,.F.);
#6292=ADVANCED_FACE('',(#1229),#5972,.F.);
#6293=ADVANCED_FACE('',(#1230),#5973,.F.);
#6294=ADVANCED_FACE('',(#1231),#5974,.F.);
#6295=ADVANCED_FACE('',(#1232),#5975,.F.);
#6296=ADVANCED_FACE('',(#1233,#666,#667,#668,#669,#670),#895,.T.);
#6297=ADVANCED_FACE('',(#1234,#671,#672,#673,#674,#675),#896,.F.);
#6298=ADVANCED_FACE('',(#1235),#5976,.T.);
#6299=ADVANCED_FACE('',(#1236,#676),#5977,.T.);
#6300=ADVANCED_FACE('',(#1237),#5978,.T.);
#6301=ADVANCED_FACE('',(#1238,#677),#897,.F.);
#6302=ADVANCED_FACE('',(#1239),#898,.T.);
#6303=ADVANCED_FACE('',(#1240),#899,.T.);
#6304=ADVANCED_FACE('',(#1241),#900,.T.);
#6305=ADVANCED_FACE('',(#1242),#901,.T.);
#6306=ADVANCED_FACE('',(#1243),#902,.T.);
#6307=ADVANCED_FACE('',(#1244),#903,.F.);
#6308=ADVANCED_FACE('',(#1245),#904,.T.);
#6309=ADVANCED_FACE('',(#1246),#905,.T.);
#6310=ADVANCED_FACE('',(#1247),#906,.T.);
#6311=ADVANCED_FACE('',(#1248),#907,.F.);
#6312=ADVANCED_FACE('',(#1249),#908,.F.);
#6313=ADVANCED_FACE('',(#1250),#909,.F.);
#6314=ADVANCED_FACE('',(#1251),#910,.F.);
#6315=ADVANCED_FACE('',(#1252),#911,.F.);
#6316=ADVANCED_FACE('',(#1253),#912,.F.);
#6317=ADVANCED_FACE('',(#1254),#913,.F.);
#6318=ADVANCED_FACE('',(#1255),#914,.F.);
#6319=ADVANCED_FACE('',(#1256,#678),#915,.T.);
#6320=ADVANCED_FACE('',(#1257),#405,.T.);
#6321=ADVANCED_FACE('',(#1258),#5979,.T.);
#6322=ADVANCED_FACE('',(#1259),#406,.T.);
#6323=ADVANCED_FACE('',(#1260),#916,.T.);
#6324=CLOSED_SHELL('',(#5980,#5981,#5982,#5983,#5984,#5985,#5986,#5987,
#5988,#5989,#5990,#5991,#5992,#5993,#5994,#5995,#5996,#5997));
#6325=CLOSED_SHELL('',(#5998,#5999,#6000,#6001,#6002,#6003));
#6326=CLOSED_SHELL('',(#6004,#6005,#6006,#6007,#6008,#6009));
#6327=CLOSED_SHELL('',(#6010,#6011,#6012,#6013,#6014,#6015));
#6328=CLOSED_SHELL('',(#6016,#6017,#6018,#6019,#6020,#6021));
#6329=CLOSED_SHELL('',(#6022,#6023,#6024,#6025,#6026,#6027,#6028,#6029,
#6030,#6031,#6032,#6033,#6034,#6035,#6036));
#6330=CLOSED_SHELL('',(#6037,#6038,#6039,#6040));
#6331=CLOSED_SHELL('',(#6041,#6042,#6043,#6044));
#6332=CLOSED_SHELL('',(#6045,#6046,#6047,#6048));
#6333=CLOSED_SHELL('',(#6049,#6050,#6051,#6052));
#6334=CLOSED_SHELL('',(#6053,#6054,#6055,#6056,#6057,#6058,#6059,#6060,
#6061,#6062,#6063,#6064,#6065,#6066,#6067));
#6335=CLOSED_SHELL('',(#6068,#6069,#6070,#6071));
#6336=CLOSED_SHELL('',(#6072,#6073,#6074,#6075));
#6337=CLOSED_SHELL('',(#6076,#6077,#6078,#6079));
#6338=CLOSED_SHELL('',(#6080,#6081,#6082,#6083));
#6339=CLOSED_SHELL('',(#6084,#6085,#6086,#6087,#6088,#6089,#6090,#6091,
#6092,#6093,#6094,#6095,#6096,#6097,#6098,#6099,#6100,#6101,#6102,#6103,
#6104,#6105,#6106,#6107,#6108,#6109,#6110,#6111,#6112,#6113,#6114,#6115,
#6116,#6117,#6118,#6119,#6120,#6121,#6122,#6123,#6124,#6125,#6126,#6127,
#6128,#6129,#6130));
#6340=CLOSED_SHELL('',(#6131,#6132,#6133,#6134,#6135,#6136,#6137,#6138,
#6139,#6140,#6141,#6142,#6143,#6144));
#6341=CLOSED_SHELL('',(#6145,#6146,#6147,#6148,#6149,#6150,#6151,#6152));
#6342=CLOSED_SHELL('',(#6153,#6154,#6155,#6156,#6157,#6158,#6159,#6160));
#6343=CLOSED_SHELL('',(#6161,#6162,#6163,#6164,#6165,#6166,#6167,#6168));
#6344=CLOSED_SHELL('',(#6169,#6170,#6171,#6172,#6173,#6174,#6175,#6176));
#6345=CLOSED_SHELL('',(#6177,#6178,#6179,#6180,#6181,#6182,#6183,#6184,
#6185,#6186,#6187,#6188,#6189,#6190,#6191,#6192,#6193,#6194,#6195,#6196,
#6197));
#6346=CLOSED_SHELL('',(#6198,#6199,#6200,#6201));
#6347=CLOSED_SHELL('',(#6202,#6203,#6204,#6205,#6206,#6207,#6208,#6209,
#6210,#6211,#6212,#6213));
#6348=CLOSED_SHELL('',(#6214,#6215,#6216,#6217,#6218,#6219,#6220,#6221,
#6222));
#6349=CLOSED_SHELL('',(#6223,#6224,#6225,#6226,#6227,#6228,#6229,#6230));
#6350=CLOSED_SHELL('',(#6231,#6232,#6233,#6234));
#6351=CLOSED_SHELL('',(#6235,#6236,#6237,#6238,#6239,#6240,#6241,#6242,
#6243,#6244,#6245));
#6352=CLOSED_SHELL('',(#6246,#6247,#6248,#6249,#6250,#6251,#6252,#6253,
#6254,#6255,#6256,#6257));
#6353=CLOSED_SHELL('',(#6258,#6259,#6260,#6261));
#6354=CLOSED_SHELL('',(#6262,#6263,#6264,#6265));
#6355=CLOSED_SHELL('',(#6266,#6267,#6268,#6269,#6270,#6271,#6272,#6273,
#6274));
#6356=CLOSED_SHELL('',(#6275,#6276,#6277,#6278,#6279,#6280,#6281,#6282,
#6283));
#6357=CLOSED_SHELL('',(#6284,#6285,#6286,#6287,#6288,#6289,#6290,#6291,
#6292,#6293,#6294,#6295,#6296,#6297,#6298,#6299,#6300,#6301));
#6358=CLOSED_SHELL('',(#6302,#6303,#6304,#6305,#6306,#6307,#6308,#6309,
#6310,#6311));
#6359=CLOSED_SHELL('',(#6312,#6313,#6314,#6315,#6316,#6317,#6318,#6319,
#6320,#6321,#6322,#6323));
#6360=DERIVED_UNIT_ELEMENT(#6424,1.);
#6361=DERIVED_UNIT_ELEMENT(#11561,-3.);
#6362=DERIVED_UNIT_ELEMENT(#6424,1.);
#6363=DERIVED_UNIT_ELEMENT(#11561,-3.);
#6364=DERIVED_UNIT_ELEMENT(#6424,1.);
#6365=DERIVED_UNIT_ELEMENT(#11561,-3.);
#6366=DERIVED_UNIT_ELEMENT(#6424,1.);
#6367=DERIVED_UNIT_ELEMENT(#11561,-3.);
#6368=DERIVED_UNIT_ELEMENT(#6424,1.);
#6369=DERIVED_UNIT_ELEMENT(#11561,-3.);
#6370=DERIVED_UNIT_ELEMENT(#6424,1.);
#6371=DERIVED_UNIT_ELEMENT(#11561,-3.);
#6372=DERIVED_UNIT_ELEMENT(#6424,1.);
#6373=DERIVED_UNIT_ELEMENT(#11561,-3.);
#6374=DERIVED_UNIT_ELEMENT(#6424,1.);
#6375=DERIVED_UNIT_ELEMENT(#11561,-3.);
#6376=DERIVED_UNIT_ELEMENT(#6424,1.);
#6377=DERIVED_UNIT_ELEMENT(#11561,-3.);
#6378=DERIVED_UNIT_ELEMENT(#6424,1.);
#6379=DERIVED_UNIT_ELEMENT(#11561,-3.);
#6380=DERIVED_UNIT_ELEMENT(#6424,1.);
#6381=DERIVED_UNIT_ELEMENT(#11561,-3.);
#6382=DERIVED_UNIT_ELEMENT(#6424,1.);
#6383=DERIVED_UNIT_ELEMENT(#11561,-3.);
#6384=DERIVED_UNIT_ELEMENT(#6424,1.);
#6385=DERIVED_UNIT_ELEMENT(#11561,-3.);
#6386=DERIVED_UNIT_ELEMENT(#6424,1.);
#6387=DERIVED_UNIT_ELEMENT(#11561,-3.);
#6388=DERIVED_UNIT_ELEMENT(#6424,1.);
#6389=DERIVED_UNIT_ELEMENT(#11561,-3.);
#6390=DERIVED_UNIT_ELEMENT(#6424,1.);
#6391=DERIVED_UNIT_ELEMENT(#11561,-3.);
#6392=DERIVED_UNIT_ELEMENT(#6424,1.);
#6393=DERIVED_UNIT_ELEMENT(#11561,-3.);
#6394=DERIVED_UNIT_ELEMENT(#6424,1.);
#6395=DERIVED_UNIT_ELEMENT(#11561,-3.);
#6396=DERIVED_UNIT_ELEMENT(#6424,1.);
#6397=DERIVED_UNIT_ELEMENT(#11561,-3.);
#6398=DERIVED_UNIT_ELEMENT(#6424,1.);
#6399=DERIVED_UNIT_ELEMENT(#11561,-3.);
#6400=DERIVED_UNIT_ELEMENT(#6424,1.);
#6401=DERIVED_UNIT_ELEMENT(#11561,-3.);
#6402=DERIVED_UNIT_ELEMENT(#6424,1.);
#6403=DERIVED_UNIT_ELEMENT(#11561,-3.);
#6404=DERIVED_UNIT_ELEMENT(#6424,1.);
#6405=DERIVED_UNIT_ELEMENT(#11561,-3.);
#6406=DERIVED_UNIT_ELEMENT(#6424,1.);
#6407=DERIVED_UNIT_ELEMENT(#11561,-3.);
#6408=DERIVED_UNIT_ELEMENT(#6424,1.);
#6409=DERIVED_UNIT_ELEMENT(#11561,-3.);
#6410=DERIVED_UNIT_ELEMENT(#6424,1.);
#6411=DERIVED_UNIT_ELEMENT(#11561,-3.);
#6412=DERIVED_UNIT_ELEMENT(#6424,1.);
#6413=DERIVED_UNIT_ELEMENT(#11561,-3.);
#6414=DERIVED_UNIT_ELEMENT(#6424,1.);
#6415=DERIVED_UNIT_ELEMENT(#11561,-3.);
#6416=DERIVED_UNIT_ELEMENT(#6424,1.);
#6417=DERIVED_UNIT_ELEMENT(#11561,-3.);
#6418=DERIVED_UNIT_ELEMENT(#6424,1.);
#6419=DERIVED_UNIT_ELEMENT(#11561,-3.);
#6420=DERIVED_UNIT_ELEMENT(#6424,1.);
#6421=DERIVED_UNIT_ELEMENT(#11561,-3.);
#6422=DERIVED_UNIT_ELEMENT(#6424,1.);
#6423=DERIVED_UNIT_ELEMENT(#11561,-3.);
#6424=(
MASS_UNIT()
NAMED_UNIT(*)
SI_UNIT(.KILO.,.GRAM.)
);
#6425=DERIVED_UNIT((#6360,#6361));
#6426=DERIVED_UNIT((#6362,#6363));
#6427=DERIVED_UNIT((#6364,#6365));
#6428=DERIVED_UNIT((#6366,#6367));
#6429=DERIVED_UNIT((#6368,#6369));
#6430=DERIVED_UNIT((#6370,#6371));
#6431=DERIVED_UNIT((#6372,#6373));
#6432=DERIVED_UNIT((#6374,#6375));
#6433=DERIVED_UNIT((#6376,#6377));
#6434=DERIVED_UNIT((#6378,#6379));
#6435=DERIVED_UNIT((#6380,#6381));
#6436=DERIVED_UNIT((#6382,#6383));
#6437=DERIVED_UNIT((#6384,#6385));
#6438=DERIVED_UNIT((#6386,#6387));
#6439=DERIVED_UNIT((#6388,#6389));
#6440=DERIVED_UNIT((#6390,#6391));
#6441=DERIVED_UNIT((#6392,#6393));
#6442=DERIVED_UNIT((#6394,#6395));
#6443=DERIVED_UNIT((#6396,#6397));
#6444=DERIVED_UNIT((#6398,#6399));
#6445=DERIVED_UNIT((#6400,#6401));
#6446=DERIVED_UNIT((#6402,#6403));
#6447=DERIVED_UNIT((#6404,#6405));
#6448=DERIVED_UNIT((#6406,#6407));
#6449=DERIVED_UNIT((#6408,#6409));
#6450=DERIVED_UNIT((#6410,#6411));
#6451=DERIVED_UNIT((#6412,#6413));
#6452=DERIVED_UNIT((#6414,#6415));
#6453=DERIVED_UNIT((#6416,#6417));
#6454=DERIVED_UNIT((#6418,#6419));
#6455=DERIVED_UNIT((#6420,#6421));
#6456=DERIVED_UNIT((#6422,#6423));
#6457=MEASURE_REPRESENTATION_ITEM('density measure',
POSITIVE_RATIO_MEASURE(7850.),#6425);
#6458=MEASURE_REPRESENTATION_ITEM('density measure',
POSITIVE_RATIO_MEASURE(7850.),#6426);
#6459=MEASURE_REPRESENTATION_ITEM('density measure',
POSITIVE_RATIO_MEASURE(7850.),#6427);
#6460=MEASURE_REPRESENTATION_ITEM('density measure',
POSITIVE_RATIO_MEASURE(7850.),#6428);
#6461=MEASURE_REPRESENTATION_ITEM('density measure',
POSITIVE_RATIO_MEASURE(7850.),#6429);
#6462=MEASURE_REPRESENTATION_ITEM('density measure',
POSITIVE_RATIO_MEASURE(7850.),#6430);
#6463=MEASURE_REPRESENTATION_ITEM('density measure',
POSITIVE_RATIO_MEASURE(7850.),#6431);
#6464=MEASURE_REPRESENTATION_ITEM('density measure',
POSITIVE_RATIO_MEASURE(7850.),#6432);
#6465=MEASURE_REPRESENTATION_ITEM('density measure',
POSITIVE_RATIO_MEASURE(7850.),#6433);
#6466=MEASURE_REPRESENTATION_ITEM('density measure',
POSITIVE_RATIO_MEASURE(7850.),#6434);
#6467=MEASURE_REPRESENTATION_ITEM('density measure',
POSITIVE_RATIO_MEASURE(7850.),#6435);
#6468=MEASURE_REPRESENTATION_ITEM('density measure',
POSITIVE_RATIO_MEASURE(7850.),#6436);
#6469=MEASURE_REPRESENTATION_ITEM('density measure',
POSITIVE_RATIO_MEASURE(7850.),#6437);
#6470=MEASURE_REPRESENTATION_ITEM('density measure',
POSITIVE_RATIO_MEASURE(7850.),#6438);
#6471=MEASURE_REPRESENTATION_ITEM('density measure',
POSITIVE_RATIO_MEASURE(7850.),#6439);
#6472=MEASURE_REPRESENTATION_ITEM('density measure',
POSITIVE_RATIO_MEASURE(7850.),#6440);
#6473=MEASURE_REPRESENTATION_ITEM('density measure',
POSITIVE_RATIO_MEASURE(7850.),#6441);
#6474=MEASURE_REPRESENTATION_ITEM('density measure',
POSITIVE_RATIO_MEASURE(7850.),#6442);
#6475=MEASURE_REPRESENTATION_ITEM('density measure',
POSITIVE_RATIO_MEASURE(7850.),#6443);
#6476=MEASURE_REPRESENTATION_ITEM('density measure',
POSITIVE_RATIO_MEASURE(7850.),#6444);
#6477=MEASURE_REPRESENTATION_ITEM('density measure',
POSITIVE_RATIO_MEASURE(7850.),#6445);
#6478=MEASURE_REPRESENTATION_ITEM('density measure',
POSITIVE_RATIO_MEASURE(7850.),#6446);
#6479=MEASURE_REPRESENTATION_ITEM('density measure',
POSITIVE_RATIO_MEASURE(7850.),#6447);
#6480=MEASURE_REPRESENTATION_ITEM('density measure',
POSITIVE_RATIO_MEASURE(7850.),#6448);
#6481=MEASURE_REPRESENTATION_ITEM('density measure',
POSITIVE_RATIO_MEASURE(7850.),#6449);
#6482=MEASURE_REPRESENTATION_ITEM('density measure',
POSITIVE_RATIO_MEASURE(7850.),#6450);
#6483=MEASURE_REPRESENTATION_ITEM('density measure',
POSITIVE_RATIO_MEASURE(7850.),#6451);
#6484=MEASURE_REPRESENTATION_ITEM('density measure',
POSITIVE_RATIO_MEASURE(7850.),#6452);
#6485=MEASURE_REPRESENTATION_ITEM('density measure',
POSITIVE_RATIO_MEASURE(7850.),#6453);
#6486=MEASURE_REPRESENTATION_ITEM('density measure',
POSITIVE_RATIO_MEASURE(7850.),#6454);
#6487=MEASURE_REPRESENTATION_ITEM('density measure',
POSITIVE_RATIO_MEASURE(7850.),#6455);
#6488=MEASURE_REPRESENTATION_ITEM('density measure',
POSITIVE_RATIO_MEASURE(7850.),#6456);
#6489=PROPERTY_DEFINITION_REPRESENTATION(#6649,#6553);
#6490=PROPERTY_DEFINITION_REPRESENTATION(#6650,#6554);
#6491=PROPERTY_DEFINITION_REPRESENTATION(#6651,#6555);
#6492=PROPERTY_DEFINITION_REPRESENTATION(#6652,#6556);
#6493=PROPERTY_DEFINITION_REPRESENTATION(#6653,#6557);
#6494=PROPERTY_DEFINITION_REPRESENTATION(#6654,#6558);
#6495=PROPERTY_DEFINITION_REPRESENTATION(#6655,#6559);
#6496=PROPERTY_DEFINITION_REPRESENTATION(#6656,#6560);
#6497=PROPERTY_DEFINITION_REPRESENTATION(#6657,#6561);
#6498=PROPERTY_DEFINITION_REPRESENTATION(#6658,#6562);
#6499=PROPERTY_DEFINITION_REPRESENTATION(#6659,#6563);
#6500=PROPERTY_DEFINITION_REPRESENTATION(#6660,#6564);
#6501=PROPERTY_DEFINITION_REPRESENTATION(#6661,#6565);
#6502=PROPERTY_DEFINITION_REPRESENTATION(#6662,#6566);
#6503=PROPERTY_DEFINITION_REPRESENTATION(#6663,#6567);
#6504=PROPERTY_DEFINITION_REPRESENTATION(#6664,#6568);
#6505=PROPERTY_DEFINITION_REPRESENTATION(#6665,#6569);
#6506=PROPERTY_DEFINITION_REPRESENTATION(#6666,#6570);
#6507=PROPERTY_DEFINITION_REPRESENTATION(#6667,#6571);
#6508=PROPERTY_DEFINITION_REPRESENTATION(#6668,#6572);
#6509=PROPERTY_DEFINITION_REPRESENTATION(#6669,#6573);
#6510=PROPERTY_DEFINITION_REPRESENTATION(#6670,#6574);
#6511=PROPERTY_DEFINITION_REPRESENTATION(#6671,#6575);
#6512=PROPERTY_DEFINITION_REPRESENTATION(#6672,#6576);
#6513=PROPERTY_DEFINITION_REPRESENTATION(#6673,#6577);
#6514=PROPERTY_DEFINITION_REPRESENTATION(#6674,#6578);
#6515=PROPERTY_DEFINITION_REPRESENTATION(#6675,#6579);
#6516=PROPERTY_DEFINITION_REPRESENTATION(#6676,#6580);
#6517=PROPERTY_DEFINITION_REPRESENTATION(#6677,#6581);
#6518=PROPERTY_DEFINITION_REPRESENTATION(#6678,#6582);
#6519=PROPERTY_DEFINITION_REPRESENTATION(#6679,#6583);
#6520=PROPERTY_DEFINITION_REPRESENTATION(#6680,#6584);
#6521=PROPERTY_DEFINITION_REPRESENTATION(#6681,#6585);
#6522=PROPERTY_DEFINITION_REPRESENTATION(#6682,#6586);
#6523=PROPERTY_DEFINITION_REPRESENTATION(#6683,#6587);
#6524=PROPERTY_DEFINITION_REPRESENTATION(#6684,#6588);
#6525=PROPERTY_DEFINITION_REPRESENTATION(#6685,#6589);
#6526=PROPERTY_DEFINITION_REPRESENTATION(#6686,#6590);
#6527=PROPERTY_DEFINITION_REPRESENTATION(#6687,#6591);
#6528=PROPERTY_DEFINITION_REPRESENTATION(#6688,#6592);
#6529=PROPERTY_DEFINITION_REPRESENTATION(#6689,#6593);
#6530=PROPERTY_DEFINITION_REPRESENTATION(#6690,#6594);
#6531=PROPERTY_DEFINITION_REPRESENTATION(#6691,#6595);
#6532=PROPERTY_DEFINITION_REPRESENTATION(#6692,#6596);
#6533=PROPERTY_DEFINITION_REPRESENTATION(#6693,#6597);
#6534=PROPERTY_DEFINITION_REPRESENTATION(#6694,#6598);
#6535=PROPERTY_DEFINITION_REPRESENTATION(#6695,#6599);
#6536=PROPERTY_DEFINITION_REPRESENTATION(#6696,#6600);
#6537=PROPERTY_DEFINITION_REPRESENTATION(#6697,#6601);
#6538=PROPERTY_DEFINITION_REPRESENTATION(#6698,#6602);
#6539=PROPERTY_DEFINITION_REPRESENTATION(#6699,#6603);
#6540=PROPERTY_DEFINITION_REPRESENTATION(#6700,#6604);
#6541=PROPERTY_DEFINITION_REPRESENTATION(#6701,#6605);
#6542=PROPERTY_DEFINITION_REPRESENTATION(#6702,#6606);
#6543=PROPERTY_DEFINITION_REPRESENTATION(#6703,#6607);
#6544=PROPERTY_DEFINITION_REPRESENTATION(#6704,#6608);
#6545=PROPERTY_DEFINITION_REPRESENTATION(#6705,#6609);
#6546=PROPERTY_DEFINITION_REPRESENTATION(#6706,#6610);
#6547=PROPERTY_DEFINITION_REPRESENTATION(#6707,#6611);
#6548=PROPERTY_DEFINITION_REPRESENTATION(#6708,#6612);
#6549=PROPERTY_DEFINITION_REPRESENTATION(#6709,#6613);
#6550=PROPERTY_DEFINITION_REPRESENTATION(#6710,#6614);
#6551=PROPERTY_DEFINITION_REPRESENTATION(#6711,#6615);
#6552=PROPERTY_DEFINITION_REPRESENTATION(#6712,#6616);
#6553=REPRESENTATION('material name',(#6617),#11525);
#6554=REPRESENTATION('density',(#6457),#11525);
#6555=REPRESENTATION('material name',(#6618),#11526);
#6556=REPRESENTATION('density',(#6458),#11526);
#6557=REPRESENTATION('material name',(#6619),#11527);
#6558=REPRESENTATION('density',(#6459),#11527);
#6559=REPRESENTATION('material name',(#6620),#11528);
#6560=REPRESENTATION('density',(#6460),#11528);
#6561=REPRESENTATION('material name',(#6621),#11529);
#6562=REPRESENTATION('density',(#6461),#11529);
#6563=REPRESENTATION('material name',(#6622),#11530);
#6564=REPRESENTATION('density',(#6462),#11530);
#6565=REPRESENTATION('material name',(#6623),#11531);
#6566=REPRESENTATION('density',(#6463),#11531);
#6567=REPRESENTATION('material name',(#6624),#11532);
#6568=REPRESENTATION('density',(#6464),#11532);
#6569=REPRESENTATION('material name',(#6625),#11533);
#6570=REPRESENTATION('density',(#6465),#11533);
#6571=REPRESENTATION('material name',(#6626),#11534);
#6572=REPRESENTATION('density',(#6466),#11534);
#6573=REPRESENTATION('material name',(#6627),#11535);
#6574=REPRESENTATION('density',(#6467),#11535);
#6575=REPRESENTATION('material name',(#6628),#11536);
#6576=REPRESENTATION('density',(#6468),#11536);
#6577=REPRESENTATION('material name',(#6629),#11537);
#6578=REPRESENTATION('density',(#6469),#11537);
#6579=REPRESENTATION('material name',(#6630),#11538);
#6580=REPRESENTATION('density',(#6470),#11538);
#6581=REPRESENTATION('material name',(#6631),#11539);
#6582=REPRESENTATION('density',(#6471),#11539);
#6583=REPRESENTATION('material name',(#6632),#11540);
#6584=REPRESENTATION('density',(#6472),#11540);
#6585=REPRESENTATION('material name',(#6633),#11541);
#6586=REPRESENTATION('density',(#6473),#11541);
#6587=REPRESENTATION('material name',(#6634),#11542);
#6588=REPRESENTATION('density',(#6474),#11542);
#6589=REPRESENTATION('material name',(#6635),#11543);
#6590=REPRESENTATION('density',(#6475),#11543);
#6591=REPRESENTATION('material name',(#6636),#11545);
#6592=REPRESENTATION('density',(#6476),#11545);
#6593=REPRESENTATION('material name',(#6637),#11546);
#6594=REPRESENTATION('density',(#6477),#11546);
#6595=REPRESENTATION('material name',(#6638),#11547);
#6596=REPRESENTATION('density',(#6478),#11547);
#6597=REPRESENTATION('material name',(#6639),#11548);
#6598=REPRESENTATION('density',(#6479),#11548);
#6599=REPRESENTATION('material name',(#6640),#11549);
#6600=REPRESENTATION('density',(#6480),#11549);
#6601=REPRESENTATION('material name',(#6641),#11551);
#6602=REPRESENTATION('density',(#6481),#11551);
#6603=REPRESENTATION('material name',(#6642),#11552);
#6604=REPRESENTATION('density',(#6482),#11552);
#6605=REPRESENTATION('material name',(#6643),#11553);
#6606=REPRESENTATION('density',(#6483),#11553);
#6607=REPRESENTATION('material name',(#6644),#11554);
#6608=REPRESENTATION('density',(#6484),#11554);
#6609=REPRESENTATION('material name',(#6645),#11555);
#6610=REPRESENTATION('density',(#6485),#11555);
#6611=REPRESENTATION('material name',(#6646),#11556);
#6612=REPRESENTATION('density',(#6486),#11556);
#6613=REPRESENTATION('material name',(#6647),#11557);
#6614=REPRESENTATION('density',(#6487),#11557);
#6615=REPRESENTATION('material name',(#6648),#11558);
#6616=REPRESENTATION('density',(#6488),#11558);
#6617=DESCRIPTIVE_REPRESENTATION_ITEM('Steel','Steel');
#6618=DESCRIPTIVE_REPRESENTATION_ITEM('Steel','Steel');
#6619=DESCRIPTIVE_REPRESENTATION_ITEM('Steel','Steel');
#6620=DESCRIPTIVE_REPRESENTATION_ITEM('Steel','Steel');
#6621=DESCRIPTIVE_REPRESENTATION_ITEM('Steel','Steel');
#6622=DESCRIPTIVE_REPRESENTATION_ITEM('Steel','Steel');
#6623=DESCRIPTIVE_REPRESENTATION_ITEM('Steel','Steel');
#6624=DESCRIPTIVE_REPRESENTATION_ITEM('Steel','Steel');
#6625=DESCRIPTIVE_REPRESENTATION_ITEM('Steel','Steel');
#6626=DESCRIPTIVE_REPRESENTATION_ITEM('Steel','Steel');
#6627=DESCRIPTIVE_REPRESENTATION_ITEM('Steel','Steel');
#6628=DESCRIPTIVE_REPRESENTATION_ITEM('Steel','Steel');
#6629=DESCRIPTIVE_REPRESENTATION_ITEM('Steel','Steel');
#6630=DESCRIPTIVE_REPRESENTATION_ITEM('Steel','Steel');
#6631=DESCRIPTIVE_REPRESENTATION_ITEM('Steel','Steel');
#6632=DESCRIPTIVE_REPRESENTATION_ITEM('Steel','Steel');
#6633=DESCRIPTIVE_REPRESENTATION_ITEM('Steel','Steel');
#6634=DESCRIPTIVE_REPRESENTATION_ITEM('Steel','Steel');
#6635=DESCRIPTIVE_REPRESENTATION_ITEM('Steel','Steel');
#6636=DESCRIPTIVE_REPRESENTATION_ITEM('Steel','Steel');
#6637=DESCRIPTIVE_REPRESENTATION_ITEM('Steel','Steel');
#6638=DESCRIPTIVE_REPRESENTATION_ITEM('Steel','Steel');
#6639=DESCRIPTIVE_REPRESENTATION_ITEM('Steel','Steel');
#6640=DESCRIPTIVE_REPRESENTATION_ITEM('Steel','Steel');
#6641=DESCRIPTIVE_REPRESENTATION_ITEM('Steel','Steel');
#6642=DESCRIPTIVE_REPRESENTATION_ITEM('Steel','Steel');
#6643=DESCRIPTIVE_REPRESENTATION_ITEM('Steel','Steel');
#6644=DESCRIPTIVE_REPRESENTATION_ITEM('Steel','Steel');
#6645=DESCRIPTIVE_REPRESENTATION_ITEM('Steel','Steel');
#6646=DESCRIPTIVE_REPRESENTATION_ITEM('Steel','Steel');
#6647=DESCRIPTIVE_REPRESENTATION_ITEM('Steel','Steel');
#6648=DESCRIPTIVE_REPRESENTATION_ITEM('Steel','Steel');
#6649=PROPERTY_DEFINITION('material property','material name',#11760);
#6650=PROPERTY_DEFINITION('material property','density of part',#11760);
#6651=PROPERTY_DEFINITION('material property','material name',#11761);
#6652=PROPERTY_DEFINITION('material property','density of part',#11761);
#6653=PROPERTY_DEFINITION('material property','material name',#11762);
#6654=PROPERTY_DEFINITION('material property','density of part',#11762);
#6655=PROPERTY_DEFINITION('material property','material name',#11763);
#6656=PROPERTY_DEFINITION('material property','density of part',#11763);
#6657=PROPERTY_DEFINITION('material property','material name',#11764);
#6658=PROPERTY_DEFINITION('material property','density of part',#11764);
#6659=PROPERTY_DEFINITION('material property','material name',#11765);
#6660=PROPERTY_DEFINITION('material property','density of part',#11765);
#6661=PROPERTY_DEFINITION('material property','material name',#11766);
#6662=PROPERTY_DEFINITION('material property','density of part',#11766);
#6663=PROPERTY_DEFINITION('material property','material name',#11767);
#6664=PROPERTY_DEFINITION('material property','density of part',#11767);
#6665=PROPERTY_DEFINITION('material property','material name',#11768);
#6666=PROPERTY_DEFINITION('material property','density of part',#11768);
#6667=PROPERTY_DEFINITION('material property','material name',#11769);
#6668=PROPERTY_DEFINITION('material property','density of part',#11769);
#6669=PROPERTY_DEFINITION('material property','material name',#11770);
#6670=PROPERTY_DEFINITION('material property','density of part',#11770);
#6671=PROPERTY_DEFINITION('material property','material name',#11771);
#6672=PROPERTY_DEFINITION('material property','density of part',#11771);
#6673=PROPERTY_DEFINITION('material property','material name',#11772);
#6674=PROPERTY_DEFINITION('material property','density of part',#11772);
#6675=PROPERTY_DEFINITION('material property','material name',#11773);
#6676=PROPERTY_DEFINITION('material property','density of part',#11773);
#6677=PROPERTY_DEFINITION('material property','material name',#11774);
#6678=PROPERTY_DEFINITION('material property','density of part',#11774);
#6679=PROPERTY_DEFINITION('material property','material name',#11775);
#6680=PROPERTY_DEFINITION('material property','density of part',#11775);
#6681=PROPERTY_DEFINITION('material property','material name',#11776);
#6682=PROPERTY_DEFINITION('material property','density of part',#11776);
#6683=PROPERTY_DEFINITION('material property','material name',#11777);
#6684=PROPERTY_DEFINITION('material property','density of part',#11777);
#6685=PROPERTY_DEFINITION('material property','material name',#11778);
#6686=PROPERTY_DEFINITION('material property','density of part',#11778);
#6687=PROPERTY_DEFINITION('material property','material name',#11780);
#6688=PROPERTY_DEFINITION('material property','density of part',#11780);
#6689=PROPERTY_DEFINITION('material property','material name',#11781);
#6690=PROPERTY_DEFINITION('material property','density of part',#11781);
#6691=PROPERTY_DEFINITION('material property','material name',#11782);
#6692=PROPERTY_DEFINITION('material property','density of part',#11782);
#6693=PROPERTY_DEFINITION('material property','material name',#11783);
#6694=PROPERTY_DEFINITION('material property','density of part',#11783);
#6695=PROPERTY_DEFINITION('material property','material name',#11784);
#6696=PROPERTY_DEFINITION('material property','density of part',#11784);
#6697=PROPERTY_DEFINITION('material property','material name',#11786);
#6698=PROPERTY_DEFINITION('material property','density of part',#11786);
#6699=PROPERTY_DEFINITION('material property','material name',#11787);
#6700=PROPERTY_DEFINITION('material property','density of part',#11787);
#6701=PROPERTY_DEFINITION('material property','material name',#11788);
#6702=PROPERTY_DEFINITION('material property','density of part',#11788);
#6703=PROPERTY_DEFINITION('material property','material name',#11789);
#6704=PROPERTY_DEFINITION('material property','density of part',#11789);
#6705=PROPERTY_DEFINITION('material property','material name',#11790);
#6706=PROPERTY_DEFINITION('material property','density of part',#11790);
#6707=PROPERTY_DEFINITION('material property','material name',#11791);
#6708=PROPERTY_DEFINITION('material property','density of part',#11791);
#6709=PROPERTY_DEFINITION('material property','material name',#11792);
#6710=PROPERTY_DEFINITION('material property','density of part',#11792);
#6711=PROPERTY_DEFINITION('material property','material name',#11793);
#6712=PROPERTY_DEFINITION('material property','density of part',#11793);
#6713=AXIS2_PLACEMENT_3D('',#9234,#7371,#7372);
#6714=AXIS2_PLACEMENT_3D('',#9235,#7373,#7374);
#6715=AXIS2_PLACEMENT_3D('',#9236,#7375,#7376);
#6716=AXIS2_PLACEMENT_3D('',#9237,#7377,#7378);
#6717=AXIS2_PLACEMENT_3D('',#9239,#7379,#7380);
#6718=AXIS2_PLACEMENT_3D('',#9242,#7382,#7383);
#6719=AXIS2_PLACEMENT_3D('',#9243,#7384,#7385);
#6720=AXIS2_PLACEMENT_3D('',#9245,#7386,#7387);
#6721=AXIS2_PLACEMENT_3D('',#9248,#7389,#7390);
#6722=AXIS2_PLACEMENT_3D('',#9249,#7391,#7392);
#6723=AXIS2_PLACEMENT_3D('',#9251,#7393,#7394);
#6724=AXIS2_PLACEMENT_3D('',#9254,#7396,#7397);
#6725=AXIS2_PLACEMENT_3D('',#9255,#7398,#7399);
#6726=AXIS2_PLACEMENT_3D('',#9257,#7400,#7401);
#6727=AXIS2_PLACEMENT_3D('',#9260,#7403,#7404);
#6728=AXIS2_PLACEMENT_3D('',#9261,#7405,#7406);
#6729=AXIS2_PLACEMENT_3D('',#9263,#7407,#7408);
#6730=AXIS2_PLACEMENT_3D('',#9266,#7410,#7411);
#6731=AXIS2_PLACEMENT_3D('',#9267,#7412,#7413);
#6732=AXIS2_PLACEMENT_3D('',#9269,#7414,#7415);
#6733=AXIS2_PLACEMENT_3D('',#9272,#7417,#7418);
#6734=AXIS2_PLACEMENT_3D('',#9273,#7419,#7420);
#6735=AXIS2_PLACEMENT_3D('',#9275,#7421,#7422);
#6736=AXIS2_PLACEMENT_3D('',#9278,#7424,#7425);
#6737=AXIS2_PLACEMENT_3D('',#9279,#7426,#7427);
#6738=AXIS2_PLACEMENT_3D('',#9281,#7428,#7429);
#6739=AXIS2_PLACEMENT_3D('',#9284,#7431,#7432);
#6740=AXIS2_PLACEMENT_3D('',#9285,#7433,#7434);
#6741=AXIS2_PLACEMENT_3D('',#9287,#7435,#7436);
#6742=AXIS2_PLACEMENT_3D('',#9290,#7438,#7439);
#6743=AXIS2_PLACEMENT_3D('',#9291,#7440,#7441);
#6744=AXIS2_PLACEMENT_3D('',#9293,#7442,#7443);
#6745=AXIS2_PLACEMENT_3D('',#9296,#7445,#7446);
#6746=AXIS2_PLACEMENT_3D('',#9297,#7447,#7448);
#6747=AXIS2_PLACEMENT_3D('',#9299,#7449,#7450);
#6748=AXIS2_PLACEMENT_3D('',#9302,#7452,#7453);
#6749=AXIS2_PLACEMENT_3D('',#9303,#7454,#7455);
#6750=AXIS2_PLACEMENT_3D('',#9305,#7456,#7457);
#6751=AXIS2_PLACEMENT_3D('',#9308,#7459,#7460);
#6752=AXIS2_PLACEMENT_3D('',#9309,#7461,#7462);
#6753=AXIS2_PLACEMENT_3D('',#9318,#7467,#7468);
#6754=AXIS2_PLACEMENT_3D('',#9324,#7472,#7473);
#6755=AXIS2_PLACEMENT_3D('',#9330,#7477,#7478);
#6756=AXIS2_PLACEMENT_3D('',#9333,#7481,#7482);
#6757=AXIS2_PLACEMENT_3D('',#9334,#7483,#7484);
#6758=AXIS2_PLACEMENT_3D('',#9335,#7485,#7486);
#6759=AXIS2_PLACEMENT_3D('',#9336,#7487,#7488);
#6760=AXIS2_PLACEMENT_3D('',#9345,#7493,#7494);
#6761=AXIS2_PLACEMENT_3D('',#9351,#7498,#7499);
#6762=AXIS2_PLACEMENT_3D('',#9357,#7503,#7504);
#6763=AXIS2_PLACEMENT_3D('',#9360,#7507,#7508);
#6764=AXIS2_PLACEMENT_3D('',#9361,#7509,#7510);
#6765=AXIS2_PLACEMENT_3D('',#9362,#7511,#7512);
#6766=AXIS2_PLACEMENT_3D('',#9363,#7513,#7514);
#6767=AXIS2_PLACEMENT_3D('',#9372,#7519,#7520);
#6768=AXIS2_PLACEMENT_3D('',#9378,#7524,#7525);
#6769=AXIS2_PLACEMENT_3D('',#9384,#7529,#7530);
#6770=AXIS2_PLACEMENT_3D('',#9387,#7533,#7534);
#6771=AXIS2_PLACEMENT_3D('',#9388,#7535,#7536);
#6772=AXIS2_PLACEMENT_3D('',#9389,#7537,#7538);
#6773=AXIS2_PLACEMENT_3D('',#9390,#7539,#7540);
#6774=AXIS2_PLACEMENT_3D('',#9399,#7545,#7546);
#6775=AXIS2_PLACEMENT_3D('',#9405,#7550,#7551);
#6776=AXIS2_PLACEMENT_3D('',#9411,#7555,#7556);
#6777=AXIS2_PLACEMENT_3D('',#9414,#7559,#7560);
#6778=AXIS2_PLACEMENT_3D('',#9415,#7561,#7562);
#6779=AXIS2_PLACEMENT_3D('',#9416,#7563,#7564);
#6780=AXIS2_PLACEMENT_3D('',#9417,#7565,#7566);
#6781=AXIS2_PLACEMENT_3D('',#9426,#7571,#7572);
#6782=AXIS2_PLACEMENT_3D('',#9432,#7576,#7577);
#6783=AXIS2_PLACEMENT_3D('',#9438,#7581,#7582);
#6784=AXIS2_PLACEMENT_3D('',#9441,#7585,#7586);
#6785=AXIS2_PLACEMENT_3D('',#9442,#7587,#7588);
#6786=AXIS2_PLACEMENT_3D('',#9443,#7589,#7590);
#6787=AXIS2_PLACEMENT_3D('',#9444,#7591,#7592);
#6788=AXIS2_PLACEMENT_3D('',#9446,#7593,#7594);
#6789=AXIS2_PLACEMENT_3D('',#9449,#7596,#7597);
#6790=AXIS2_PLACEMENT_3D('',#9450,#7598,#7599);
#6791=AXIS2_PLACEMENT_3D('',#9452,#7600,#7601);
#6792=AXIS2_PLACEMENT_3D('',#9455,#7603,#7604);
#6793=AXIS2_PLACEMENT_3D('',#9456,#7605,#7606);
#6794=AXIS2_PLACEMENT_3D('',#9458,#7607,#7608);
#6795=AXIS2_PLACEMENT_3D('',#9461,#7610,#7611);
#6796=AXIS2_PLACEMENT_3D('',#9462,#7612,#7613);
#6797=AXIS2_PLACEMENT_3D('',#9464,#7614,#7615);
#6798=AXIS2_PLACEMENT_3D('',#9467,#7617,#7618);
#6799=AXIS2_PLACEMENT_3D('',#9468,#7619,#7620);
#6800=AXIS2_PLACEMENT_3D('',#9470,#7621,#7622);
#6801=AXIS2_PLACEMENT_3D('',#9473,#7624,#7625);
#6802=AXIS2_PLACEMENT_3D('',#9474,#7626,#7627);
#6803=AXIS2_PLACEMENT_3D('',#9476,#7628,#7629);
#6804=AXIS2_PLACEMENT_3D('',#9479,#7631,#7632);
#6805=AXIS2_PLACEMENT_3D('',#9480,#7633,#7634);
#6806=AXIS2_PLACEMENT_3D('',#9482,#7635,#7636);
#6807=AXIS2_PLACEMENT_3D('',#9485,#7638,#7639);
#6808=AXIS2_PLACEMENT_3D('',#9486,#7640,#7641);
#6809=AXIS2_PLACEMENT_3D('',#9495,#7646,#7647);
#6810=AXIS2_PLACEMENT_3D('',#9501,#7651,#7652);
#6811=AXIS2_PLACEMENT_3D('',#9510,#7657,#7658);
#6812=AXIS2_PLACEMENT_3D('',#9515,#7662,#7663);
#6813=AXIS2_PLACEMENT_3D('',#9520,#7667,#7668);
#6814=AXIS2_PLACEMENT_3D('',#9522,#7670,#7671);
#6815=AXIS2_PLACEMENT_3D('',#9523,#7672,#7673);
#6816=AXIS2_PLACEMENT_3D('',#9524,#7674,#7675);
#6817=AXIS2_PLACEMENT_3D('',#9525,#7676,#7677);
#6818=AXIS2_PLACEMENT_3D('',#9527,#7678,#7679);
#6819=AXIS2_PLACEMENT_3D('',#9530,#7681,#7682);
#6820=AXIS2_PLACEMENT_3D('',#9531,#7683,#7684);
#6821=AXIS2_PLACEMENT_3D('',#9533,#7685,#7686);
#6822=AXIS2_PLACEMENT_3D('',#9536,#7688,#7689);
#6823=AXIS2_PLACEMENT_3D('',#9537,#7690,#7691);
#6824=AXIS2_PLACEMENT_3D('',#9538,#7692,#7693);
#6825=AXIS2_PLACEMENT_3D('',#9539,#7694,#7695);
#6826=AXIS2_PLACEMENT_3D('',#9540,#7696,#7697);
#6827=AXIS2_PLACEMENT_3D('',#9542,#7698,#7699);
#6828=AXIS2_PLACEMENT_3D('',#9545,#7701,#7702);
#6829=AXIS2_PLACEMENT_3D('',#9546,#7703,#7704);
#6830=AXIS2_PLACEMENT_3D('',#9548,#7705,#7706);
#6831=AXIS2_PLACEMENT_3D('',#9551,#7708,#7709);
#6832=AXIS2_PLACEMENT_3D('',#9552,#7710,#7711);
#6833=AXIS2_PLACEMENT_3D('',#9553,#7712,#7713);
#6834=AXIS2_PLACEMENT_3D('',#9554,#7714,#7715);
#6835=AXIS2_PLACEMENT_3D('',#9555,#7716,#7717);
#6836=AXIS2_PLACEMENT_3D('',#9557,#7718,#7719);
#6837=AXIS2_PLACEMENT_3D('',#9560,#7721,#7722);
#6838=AXIS2_PLACEMENT_3D('',#9561,#7723,#7724);
#6839=AXIS2_PLACEMENT_3D('',#9563,#7725,#7726);
#6840=AXIS2_PLACEMENT_3D('',#9566,#7728,#7729);
#6841=AXIS2_PLACEMENT_3D('',#9567,#7730,#7731);
#6842=AXIS2_PLACEMENT_3D('',#9568,#7732,#7733);
#6843=AXIS2_PLACEMENT_3D('',#9569,#7734,#7735);
#6844=AXIS2_PLACEMENT_3D('',#9570,#7736,#7737);
#6845=AXIS2_PLACEMENT_3D('',#9572,#7738,#7739);
#6846=AXIS2_PLACEMENT_3D('',#9575,#7741,#7742);
#6847=AXIS2_PLACEMENT_3D('',#9576,#7743,#7744);
#6848=AXIS2_PLACEMENT_3D('',#9578,#7745,#7746);
#6849=AXIS2_PLACEMENT_3D('',#9581,#7748,#7749);
#6850=AXIS2_PLACEMENT_3D('',#9582,#7750,#7751);
#6851=AXIS2_PLACEMENT_3D('',#9583,#7752,#7753);
#6852=AXIS2_PLACEMENT_3D('',#9584,#7754,#7755);
#6853=AXIS2_PLACEMENT_3D('',#9585,#7756,#7757);
#6854=AXIS2_PLACEMENT_3D('',#9587,#7758,#7759);
#6855=AXIS2_PLACEMENT_3D('',#9590,#7761,#7762);
#6856=AXIS2_PLACEMENT_3D('',#9591,#7763,#7764);
#6857=AXIS2_PLACEMENT_3D('',#9593,#7765,#7766);
#6858=AXIS2_PLACEMENT_3D('',#9596,#7768,#7769);
#6859=AXIS2_PLACEMENT_3D('',#9597,#7770,#7771);
#6860=AXIS2_PLACEMENT_3D('',#9599,#7772,#7773);
#6861=AXIS2_PLACEMENT_3D('',#9602,#7775,#7776);
#6862=AXIS2_PLACEMENT_3D('',#9603,#7777,#7778);
#6863=AXIS2_PLACEMENT_3D('',#9605,#7779,#7780);
#6864=AXIS2_PLACEMENT_3D('',#9608,#7782,#7783);
#6865=AXIS2_PLACEMENT_3D('',#9609,#7784,#7785);
#6866=AXIS2_PLACEMENT_3D('',#9611,#7786,#7787);
#6867=AXIS2_PLACEMENT_3D('',#9614,#7789,#7790);
#6868=AXIS2_PLACEMENT_3D('',#9615,#7791,#7792);
#6869=AXIS2_PLACEMENT_3D('',#9617,#7793,#7794);
#6870=AXIS2_PLACEMENT_3D('',#9620,#7796,#7797);
#6871=AXIS2_PLACEMENT_3D('',#9621,#7798,#7799);
#6872=AXIS2_PLACEMENT_3D('',#9623,#7800,#7801);
#6873=AXIS2_PLACEMENT_3D('',#9626,#7803,#7804);
#6874=AXIS2_PLACEMENT_3D('',#9627,#7805,#7806);
#6875=AXIS2_PLACEMENT_3D('',#9636,#7811,#7812);
#6876=AXIS2_PLACEMENT_3D('',#9642,#7816,#7817);
#6877=AXIS2_PLACEMENT_3D('',#9651,#7822,#7823);
#6878=AXIS2_PLACEMENT_3D('',#9656,#7827,#7828);
#6879=AXIS2_PLACEMENT_3D('',#9661,#7832,#7833);
#6880=AXIS2_PLACEMENT_3D('',#9663,#7835,#7836);
#6881=AXIS2_PLACEMENT_3D('',#9664,#7837,#7838);
#6882=AXIS2_PLACEMENT_3D('',#9665,#7839,#7840);
#6883=AXIS2_PLACEMENT_3D('',#9666,#7841,#7842);
#6884=AXIS2_PLACEMENT_3D('',#9668,#7843,#7844);
#6885=AXIS2_PLACEMENT_3D('',#9671,#7846,#7847);
#6886=AXIS2_PLACEMENT_3D('',#9672,#7848,#7849);
#6887=AXIS2_PLACEMENT_3D('',#9674,#7850,#7851);
#6888=AXIS2_PLACEMENT_3D('',#9677,#7853,#7854);
#6889=AXIS2_PLACEMENT_3D('',#9678,#7855,#7856);
#6890=AXIS2_PLACEMENT_3D('',#9679,#7857,#7858);
#6891=AXIS2_PLACEMENT_3D('',#9680,#7859,#7860);
#6892=AXIS2_PLACEMENT_3D('',#9681,#7861,#7862);
#6893=AXIS2_PLACEMENT_3D('',#9683,#7863,#7864);
#6894=AXIS2_PLACEMENT_3D('',#9686,#7866,#7867);
#6895=AXIS2_PLACEMENT_3D('',#9687,#7868,#7869);
#6896=AXIS2_PLACEMENT_3D('',#9689,#7870,#7871);
#6897=AXIS2_PLACEMENT_3D('',#9692,#7873,#7874);
#6898=AXIS2_PLACEMENT_3D('',#9693,#7875,#7876);
#6899=AXIS2_PLACEMENT_3D('',#9694,#7877,#7878);
#6900=AXIS2_PLACEMENT_3D('',#9695,#7879,#7880);
#6901=AXIS2_PLACEMENT_3D('',#9696,#7881,#7882);
#6902=AXIS2_PLACEMENT_3D('',#9698,#7883,#7884);
#6903=AXIS2_PLACEMENT_3D('',#9701,#7886,#7887);
#6904=AXIS2_PLACEMENT_3D('',#9702,#7888,#7889);
#6905=AXIS2_PLACEMENT_3D('',#9704,#7890,#7891);
#6906=AXIS2_PLACEMENT_3D('',#9707,#7893,#7894);
#6907=AXIS2_PLACEMENT_3D('',#9708,#7895,#7896);
#6908=AXIS2_PLACEMENT_3D('',#9709,#7897,#7898);
#6909=AXIS2_PLACEMENT_3D('',#9710,#7899,#7900);
#6910=AXIS2_PLACEMENT_3D('',#9711,#7901,#7902);
#6911=AXIS2_PLACEMENT_3D('',#9713,#7903,#7904);
#6912=AXIS2_PLACEMENT_3D('',#9716,#7906,#7907);
#6913=AXIS2_PLACEMENT_3D('',#9717,#7908,#7909);
#6914=AXIS2_PLACEMENT_3D('',#9719,#7910,#7911);
#6915=AXIS2_PLACEMENT_3D('',#9722,#7913,#7914);
#6916=AXIS2_PLACEMENT_3D('',#9723,#7915,#7916);
#6917=AXIS2_PLACEMENT_3D('',#9724,#7917,#7918);
#6918=AXIS2_PLACEMENT_3D('',#9725,#7919,#7920);
#6919=AXIS2_PLACEMENT_3D('',#9726,#7921,#7922);
#6920=AXIS2_PLACEMENT_3D('',#9735,#7927,#7928);
#6921=AXIS2_PLACEMENT_3D('',#9741,#7932,#7933);
#6922=AXIS2_PLACEMENT_3D('',#9747,#7937,#7938);
#6923=AXIS2_PLACEMENT_3D('',#9753,#7942,#7943);
#6924=AXIS2_PLACEMENT_3D('',#9759,#7947,#7948);
#6925=AXIS2_PLACEMENT_3D('',#9765,#7952,#7953);
#6926=AXIS2_PLACEMENT_3D('',#9771,#7957,#7958);
#6927=AXIS2_PLACEMENT_3D('',#9777,#7962,#7963);
#6928=AXIS2_PLACEMENT_3D('',#9783,#7967,#7968);
#6929=AXIS2_PLACEMENT_3D('',#9792,#7973,#7974);
#6930=AXIS2_PLACEMENT_3D('',#9798,#7978,#7979);
#6931=AXIS2_PLACEMENT_3D('',#9804,#7983,#7984);
#6932=AXIS2_PLACEMENT_3D('',#9810,#7988,#7989);
#6933=AXIS2_PLACEMENT_3D('',#9816,#7993,#7994);
#6934=AXIS2_PLACEMENT_3D('',#9822,#7998,#7999);
#6935=AXIS2_PLACEMENT_3D('',#9828,#8003,#8004);
#6936=AXIS2_PLACEMENT_3D('',#9834,#8008,#8009);
#6937=AXIS2_PLACEMENT_3D('',#9840,#8013,#8014);
#6938=AXIS2_PLACEMENT_3D('',#9849,#8019,#8020);
#6939=AXIS2_PLACEMENT_3D('',#9855,#8024,#8025);
#6940=AXIS2_PLACEMENT_3D('',#9861,#8029,#8030);
#6941=AXIS2_PLACEMENT_3D('',#9867,#8034,#8035);
#6942=AXIS2_PLACEMENT_3D('',#9873,#8039,#8040);
#6943=AXIS2_PLACEMENT_3D('',#9879,#8044,#8045);
#6944=AXIS2_PLACEMENT_3D('',#9885,#8049,#8050);
#6945=AXIS2_PLACEMENT_3D('',#9891,#8054,#8055);
#6946=AXIS2_PLACEMENT_3D('',#9897,#8059,#8060);
#6947=AXIS2_PLACEMENT_3D('',#9906,#8065,#8066);
#6948=AXIS2_PLACEMENT_3D('',#9912,#8070,#8071);
#6949=AXIS2_PLACEMENT_3D('',#9918,#8075,#8076);
#6950=AXIS2_PLACEMENT_3D('',#9924,#8080,#8081);
#6951=AXIS2_PLACEMENT_3D('',#9930,#8085,#8086);
#6952=AXIS2_PLACEMENT_3D('',#9936,#8090,#8091);
#6953=AXIS2_PLACEMENT_3D('',#9942,#8095,#8096);
#6954=AXIS2_PLACEMENT_3D('',#9948,#8100,#8101);
#6955=AXIS2_PLACEMENT_3D('',#9954,#8105,#8106);
#6956=AXIS2_PLACEMENT_3D('',#9956,#8107,#8108);
#6957=AXIS2_PLACEMENT_3D('',#9959,#8110,#8111);
#6958=AXIS2_PLACEMENT_3D('',#9960,#8112,#8113);
#6959=AXIS2_PLACEMENT_3D('',#9966,#8117,#8118);
#6960=AXIS2_PLACEMENT_3D('',#9972,#8122,#8123);
#6961=AXIS2_PLACEMENT_3D('',#9975,#8126,#8127);
#6962=AXIS2_PLACEMENT_3D('',#9981,#8131,#8132);
#6963=AXIS2_PLACEMENT_3D('',#9984,#8135,#8136);
#6964=AXIS2_PLACEMENT_3D('',#9990,#8140,#8141);
#6965=AXIS2_PLACEMENT_3D('',#9993,#8144,#8145);
#6966=AXIS2_PLACEMENT_3D('',#9996,#8148,#8149);
#6967=AXIS2_PLACEMENT_3D('',#9997,#8150,#8151);
#6968=AXIS2_PLACEMENT_3D('',#9998,#8152,#8153);
#6969=AXIS2_PLACEMENT_3D('',#9999,#8154,#8155);
#6970=AXIS2_PLACEMENT_3D('',#10008,#8160,#8161);
#6971=AXIS2_PLACEMENT_3D('',#10014,#8165,#8166);
#6972=AXIS2_PLACEMENT_3D('',#10021,#8170,#8171);
#6973=AXIS2_PLACEMENT_3D('',#10022,#8172,#8173);
#6974=AXIS2_PLACEMENT_3D('',#10036,#8181,#8182);
#6975=AXIS2_PLACEMENT_3D('',#10040,#8185,#8186);
#6976=AXIS2_PLACEMENT_3D('',#10044,#8189,#8190);
#6977=AXIS2_PLACEMENT_3D('',#10054,#8196,#8197);
#6978=AXIS2_PLACEMENT_3D('',#10056,#8199,#8200);
#6979=AXIS2_PLACEMENT_3D('',#10060,#8202,#8203);
#6980=AXIS2_PLACEMENT_3D('',#10062,#8205,#8206);
#6981=AXIS2_PLACEMENT_3D('',#10064,#8207,#8208);
#6982=AXIS2_PLACEMENT_3D('',#10067,#8210,#8211);
#6983=AXIS2_PLACEMENT_3D('',#10069,#8212,#8213);
#6984=AXIS2_PLACEMENT_3D('',#10070,#8214,#8215);
#6985=AXIS2_PLACEMENT_3D('',#10071,#8216,#8217);
#6986=AXIS2_PLACEMENT_3D('',#10073,#8219,#8220);
#6987=AXIS2_PLACEMENT_3D('',#10075,#8222,#8223);
#6988=AXIS2_PLACEMENT_3D('',#10077,#8225,#8226);
#6989=AXIS2_PLACEMENT_3D('',#10078,#8227,#8228);
#6990=AXIS2_PLACEMENT_3D('',#10079,#8229,#8230);
#6991=AXIS2_PLACEMENT_3D('',#10088,#8235,#8236);
#6992=AXIS2_PLACEMENT_3D('',#10094,#8240,#8241);
#6993=AXIS2_PLACEMENT_3D('',#10100,#8245,#8246);
#6994=AXIS2_PLACEMENT_3D('',#10106,#8250,#8251);
#6995=AXIS2_PLACEMENT_3D('',#10112,#8255,#8256);
#6996=AXIS2_PLACEMENT_3D('',#10115,#8259,#8260);
#6997=AXIS2_PLACEMENT_3D('',#10116,#8261,#8262);
#6998=AXIS2_PLACEMENT_3D('',#10117,#8263,#8264);
#6999=AXIS2_PLACEMENT_3D('',#10119,#8265,#8266);
#7000=AXIS2_PLACEMENT_3D('',#10120,#8267,#8268);
#7001=AXIS2_PLACEMENT_3D('',#10122,#8269,#8270);
#7002=AXIS2_PLACEMENT_3D('',#10123,#8271,#8272);
#7003=AXIS2_PLACEMENT_3D('',#10125,#8273,#8274);
#7004=AXIS2_PLACEMENT_3D('',#10127,#8276,#8277);
#7005=AXIS2_PLACEMENT_3D('',#10129,#8278,#8279);
#7006=AXIS2_PLACEMENT_3D('',#10131,#8281,#8282);
#7007=AXIS2_PLACEMENT_3D('',#10133,#8283,#8284);
#7008=AXIS2_PLACEMENT_3D('',#10135,#8286,#8287);
#7009=AXIS2_PLACEMENT_3D('',#10137,#8288,#8289);
#7010=AXIS2_PLACEMENT_3D('',#10138,#8290,#8291);
#7011=AXIS2_PLACEMENT_3D('',#10140,#8292,#8293);
#7012=AXIS2_PLACEMENT_3D('',#10142,#8295,#8296);
#7013=AXIS2_PLACEMENT_3D('',#10144,#8298,#8299);
#7014=AXIS2_PLACEMENT_3D('',#10145,#8300,#8301);
#7015=AXIS2_PLACEMENT_3D('',#10154,#8306,#8307);
#7016=AXIS2_PLACEMENT_3D('',#10160,#8311,#8312);
#7017=AXIS2_PLACEMENT_3D('',#10166,#8316,#8317);
#7018=AXIS2_PLACEMENT_3D('',#10172,#8321,#8322);
#7019=AXIS2_PLACEMENT_3D('',#10178,#8326,#8327);
#7020=AXIS2_PLACEMENT_3D('',#10181,#8330,#8331);
#7021=AXIS2_PLACEMENT_3D('',#10182,#8332,#8333);
#7022=AXIS2_PLACEMENT_3D('',#10183,#8334,#8335);
#7023=AXIS2_PLACEMENT_3D('',#10185,#8336,#8337);
#7024=AXIS2_PLACEMENT_3D('',#10186,#8338,#8339);
#7025=AXIS2_PLACEMENT_3D('',#10188,#8340,#8341);
#7026=AXIS2_PLACEMENT_3D('',#10189,#8342,#8343);
#7027=AXIS2_PLACEMENT_3D('',#10191,#8344,#8345);
#7028=AXIS2_PLACEMENT_3D('',#10193,#8347,#8348);
#7029=AXIS2_PLACEMENT_3D('',#10195,#8349,#8350);
#7030=AXIS2_PLACEMENT_3D('',#10197,#8352,#8353);
#7031=AXIS2_PLACEMENT_3D('',#10199,#8354,#8355);
#7032=AXIS2_PLACEMENT_3D('',#10201,#8357,#8358);
#7033=AXIS2_PLACEMENT_3D('',#10203,#8359,#8360);
#7034=AXIS2_PLACEMENT_3D('',#10204,#8361,#8362);
#7035=AXIS2_PLACEMENT_3D('',#10206,#8363,#8364);
#7036=AXIS2_PLACEMENT_3D('',#10208,#8366,#8367);
#7037=AXIS2_PLACEMENT_3D('',#10210,#8369,#8370);
#7038=AXIS2_PLACEMENT_3D('',#10211,#8371,#8372);
#7039=AXIS2_PLACEMENT_3D('',#10212,#8373,#8374);
#7040=AXIS2_PLACEMENT_3D('',#10214,#8375,#8376);
#7041=AXIS2_PLACEMENT_3D('',#10217,#8378,#8379);
#7042=AXIS2_PLACEMENT_3D('',#10218,#8380,#8381);
#7043=AXIS2_PLACEMENT_3D('',#10220,#8382,#8383);
#7044=AXIS2_PLACEMENT_3D('',#10223,#8385,#8386);
#7045=AXIS2_PLACEMENT_3D('',#10224,#8387,#8388);
#7046=AXIS2_PLACEMENT_3D('',#10227,#8389,#8390);
#7047=AXIS2_PLACEMENT_3D('',#10228,#8391,#8392);
#7048=AXIS2_PLACEMENT_3D('',#10230,#8393,#8394);
#7049=AXIS2_PLACEMENT_3D('',#10233,#8396,#8397);
#7050=AXIS2_PLACEMENT_3D('',#10234,#8398,#8399);
#7051=AXIS2_PLACEMENT_3D('',#10236,#8400,#8401);
#7052=AXIS2_PLACEMENT_3D('',#10239,#8403,#8404);
#7053=AXIS2_PLACEMENT_3D('',#10240,#8405,#8406);
#7054=AXIS2_PLACEMENT_3D('',#10241,#8407,#8408);
#7055=AXIS2_PLACEMENT_3D('',#10242,#8409,#8410);
#7056=AXIS2_PLACEMENT_3D('',#10244,#8411,#8412);
#7057=AXIS2_PLACEMENT_3D('',#10247,#8414,#8415);
#7058=AXIS2_PLACEMENT_3D('',#10248,#8416,#8417);
#7059=AXIS2_PLACEMENT_3D('',#10250,#8418,#8419);
#7060=AXIS2_PLACEMENT_3D('',#10253,#8421,#8422);
#7061=AXIS2_PLACEMENT_3D('',#10254,#8423,#8424);
#7062=AXIS2_PLACEMENT_3D('',#10256,#8425,#8426);
#7063=AXIS2_PLACEMENT_3D('',#10259,#8428,#8429);
#7064=AXIS2_PLACEMENT_3D('',#10260,#8430,#8431);
#7065=AXIS2_PLACEMENT_3D('',#10262,#8432,#8433);
#7066=AXIS2_PLACEMENT_3D('',#10265,#8435,#8436);
#7067=AXIS2_PLACEMENT_3D('',#10266,#8437,#8438);
#7068=AXIS2_PLACEMENT_3D('',#10275,#8443,#8444);
#7069=AXIS2_PLACEMENT_3D('',#10281,#8448,#8449);
#7070=AXIS2_PLACEMENT_3D('',#10287,#8453,#8454);
#7071=AXIS2_PLACEMENT_3D('',#10293,#8458,#8459);
#7072=AXIS2_PLACEMENT_3D('',#10299,#8463,#8464);
#7073=AXIS2_PLACEMENT_3D('',#10305,#8468,#8469);
#7074=AXIS2_PLACEMENT_3D('',#10311,#8473,#8474);
#7075=AXIS2_PLACEMENT_3D('',#10314,#8477,#8478);
#7076=AXIS2_PLACEMENT_3D('',#10315,#8479,#8480);
#7077=AXIS2_PLACEMENT_3D('',#10316,#8481,#8482);
#7078=AXIS2_PLACEMENT_3D('',#10317,#8483,#8484);
#7079=AXIS2_PLACEMENT_3D('',#10319,#8485,#8486);
#7080=AXIS2_PLACEMENT_3D('',#10322,#8488,#8489);
#7081=AXIS2_PLACEMENT_3D('',#10323,#8490,#8491);
#7082=AXIS2_PLACEMENT_3D('',#10325,#8492,#8493);
#7083=AXIS2_PLACEMENT_3D('',#10326,#8494,#8495);
#7084=AXIS2_PLACEMENT_3D('',#10329,#8496,#8497);
#7085=AXIS2_PLACEMENT_3D('',#10331,#8498,#8499);
#7086=AXIS2_PLACEMENT_3D('',#10332,#8500,#8501);
#7087=AXIS2_PLACEMENT_3D('',#10333,#8502,#8503);
#7088=AXIS2_PLACEMENT_3D('',#10411,#8505,#8506);
#7089=AXIS2_PLACEMENT_3D('',#10489,#8508,#8509);
#7090=AXIS2_PLACEMENT_3D('',#10491,#8510,#8511);
#7091=AXIS2_PLACEMENT_3D('',#10494,#8513,#8514);
#7092=AXIS2_PLACEMENT_3D('',#10659,#8515,#8516);
#7093=AXIS2_PLACEMENT_3D('',#10696,#8518,#8519);
#7094=AXIS2_PLACEMENT_3D('',#10733,#8521,#8522);
#7095=AXIS2_PLACEMENT_3D('',#10770,#8524,#8525);
#7096=AXIS2_PLACEMENT_3D('',#10807,#8527,#8528);
#7097=AXIS2_PLACEMENT_3D('',#10809,#8529,#8530);
#7098=AXIS2_PLACEMENT_3D('',#10810,#8531,#8532);
#7099=AXIS2_PLACEMENT_3D('',#10812,#8533,#8534);
#7100=AXIS2_PLACEMENT_3D('',#10813,#8535,#8536);
#7101=AXIS2_PLACEMENT_3D('',#10815,#8537,#8538);
#7102=AXIS2_PLACEMENT_3D('',#10817,#8540,#8541);
#7103=AXIS2_PLACEMENT_3D('',#10819,#8542,#8543);
#7104=AXIS2_PLACEMENT_3D('',#10820,#8544,#8545);
#7105=AXIS2_PLACEMENT_3D('',#10822,#8547,#8548);
#7106=AXIS2_PLACEMENT_3D('',#10823,#8549,#8550);
#7107=AXIS2_PLACEMENT_3D('',#10824,#8551,#8552);
#7108=AXIS2_PLACEMENT_3D('',#10825,#8553,#8554);
#7109=AXIS2_PLACEMENT_3D('',#10827,#8555,#8556);
#7110=AXIS2_PLACEMENT_3D('',#10828,#8557,#8558);
#7111=AXIS2_PLACEMENT_3D('',#10830,#8559,#8560);
#7112=AXIS2_PLACEMENT_3D('',#10832,#8562,#8563);
#7113=AXIS2_PLACEMENT_3D('',#10834,#8564,#8565);
#7114=AXIS2_PLACEMENT_3D('',#10836,#8567,#8568);
#7115=AXIS2_PLACEMENT_3D('',#10838,#8569,#8570);
#7116=AXIS2_PLACEMENT_3D('',#10840,#8572,#8573);
#7117=AXIS2_PLACEMENT_3D('',#10842,#8574,#8575);
#7118=AXIS2_PLACEMENT_3D('',#10843,#8576,#8577);
#7119=AXIS2_PLACEMENT_3D('',#10845,#8578,#8579);
#7120=AXIS2_PLACEMENT_3D('',#10847,#8581,#8582);
#7121=AXIS2_PLACEMENT_3D('',#10849,#8583,#8584);
#7122=AXIS2_PLACEMENT_3D('',#10851,#8586,#8587);
#7123=AXIS2_PLACEMENT_3D('',#10853,#8588,#8589);
#7124=AXIS2_PLACEMENT_3D('',#10855,#8591,#8592);
#7125=AXIS2_PLACEMENT_3D('',#10856,#8593,#8594);
#7126=AXIS2_PLACEMENT_3D('',#10865,#8599,#8600);
#7127=AXIS2_PLACEMENT_3D('',#10871,#8604,#8605);
#7128=AXIS2_PLACEMENT_3D('',#10877,#8609,#8610);
#7129=AXIS2_PLACEMENT_3D('',#10883,#8614,#8615);
#7130=AXIS2_PLACEMENT_3D('',#10889,#8619,#8620);
#7131=AXIS2_PLACEMENT_3D('',#10892,#8623,#8624);
#7132=AXIS2_PLACEMENT_3D('',#10893,#8625,#8626);
#7133=AXIS2_PLACEMENT_3D('',#10894,#8627,#8628);
#7134=AXIS2_PLACEMENT_3D('',#10895,#8629,#8630);
#7135=AXIS2_PLACEMENT_3D('',#10897,#8631,#8632);
#7136=AXIS2_PLACEMENT_3D('',#10900,#8634,#8635);
#7137=AXIS2_PLACEMENT_3D('',#10901,#8636,#8637);
#7138=AXIS2_PLACEMENT_3D('',#10903,#8638,#8639);
#7139=AXIS2_PLACEMENT_3D('',#10906,#8641,#8642);
#7140=AXIS2_PLACEMENT_3D('',#10907,#8643,#8644);
#7141=AXIS2_PLACEMENT_3D('',#10908,#8645,#8646);
#7142=AXIS2_PLACEMENT_3D('',#10909,#8647,#8648);
#7143=AXIS2_PLACEMENT_3D('',#10910,#8649,#8650);
#7144=AXIS2_PLACEMENT_3D('',#10922,#8652,#8653);
#7145=AXIS2_PLACEMENT_3D('',#10938,#8654,#8655);
#7146=AXIS2_PLACEMENT_3D('',#10940,#8656,#8657);
#7147=AXIS2_PLACEMENT_3D('',#10966,#8659,#8660);
#7148=AXIS2_PLACEMENT_3D('',#10969,#8663,#8664);
#7149=AXIS2_PLACEMENT_3D('',#10971,#8666,#8667);
#7150=AXIS2_PLACEMENT_3D('',#10973,#8669,#8670);
#7151=AXIS2_PLACEMENT_3D('',#10975,#8671,#8672);
#7152=AXIS2_PLACEMENT_3D('',#10978,#8674,#8675);
#7153=AXIS2_PLACEMENT_3D('',#10979,#8676,#8677);
#7154=AXIS2_PLACEMENT_3D('',#10981,#8679,#8680);
#7155=AXIS2_PLACEMENT_3D('',#10983,#8682,#8683);
#7156=AXIS2_PLACEMENT_3D('',#10984,#8684,#8685);
#7157=AXIS2_PLACEMENT_3D('',#10985,#8686,#8687);
#7158=AXIS2_PLACEMENT_3D('',#10986,#8688,#8689);
#7159=AXIS2_PLACEMENT_3D('',#10987,#8690,#8691);
#7160=AXIS2_PLACEMENT_3D('',#10988,#8692,#8693);
#7161=AXIS2_PLACEMENT_3D('',#10989,#8694,#8695);
#7162=AXIS2_PLACEMENT_3D('',#10990,#8696,#8697);
#7163=AXIS2_PLACEMENT_3D('',#10991,#8698,#8699);
#7164=AXIS2_PLACEMENT_3D('',#10992,#8700,#8701);
#7165=AXIS2_PLACEMENT_3D('',#10993,#8702,#8703);
#7166=AXIS2_PLACEMENT_3D('',#10994,#8704,#8705);
#7167=AXIS2_PLACEMENT_3D('',#10995,#8706,#8707);
#7168=AXIS2_PLACEMENT_3D('',#10996,#8708,#8709);
#7169=AXIS2_PLACEMENT_3D('',#10997,#8710,#8711);
#7170=AXIS2_PLACEMENT_3D('',#10998,#8712,#8713);
#7171=AXIS2_PLACEMENT_3D('',#10999,#8714,#8715);
#7172=AXIS2_PLACEMENT_3D('',#11000,#8716,#8717);
#7173=AXIS2_PLACEMENT_3D('',#11001,#8718,#8719);
#7174=AXIS2_PLACEMENT_3D('',#11002,#8720,#8721);
#7175=AXIS2_PLACEMENT_3D('',#11003,#8722,#8723);
#7176=AXIS2_PLACEMENT_3D('',#11004,#8724,#8725);
#7177=AXIS2_PLACEMENT_3D('',#11005,#8726,#8727);
#7178=AXIS2_PLACEMENT_3D('',#11006,#8728,#8729);
#7179=AXIS2_PLACEMENT_3D('',#11007,#8730,#8731);
#7180=AXIS2_PLACEMENT_3D('',#11008,#8732,#8733);
#7181=AXIS2_PLACEMENT_3D('',#11009,#8734,#8735);
#7182=AXIS2_PLACEMENT_3D('',#11010,#8736,#8737);
#7183=AXIS2_PLACEMENT_3D('',#11011,#8738,#8739);
#7184=AXIS2_PLACEMENT_3D('',#11012,#8740,#8741);
#7185=AXIS2_PLACEMENT_3D('',#11013,#8742,#8743);
#7186=AXIS2_PLACEMENT_3D('',#11014,#8744,#8745);
#7187=AXIS2_PLACEMENT_3D('',#11015,#8746,#8747);
#7188=AXIS2_PLACEMENT_3D('',#11016,#8748,#8749);
#7189=AXIS2_PLACEMENT_3D('',#11017,#8750,#8751);
#7190=AXIS2_PLACEMENT_3D('',#11018,#8752,#8753);
#7191=AXIS2_PLACEMENT_3D('',#11019,#8754,#8755);
#7192=AXIS2_PLACEMENT_3D('',#11020,#8756,#8757);
#7193=AXIS2_PLACEMENT_3D('',#11021,#8758,#8759);
#7194=AXIS2_PLACEMENT_3D('',#11022,#8760,#8761);
#7195=AXIS2_PLACEMENT_3D('',#11023,#8762,#8763);
#7196=AXIS2_PLACEMENT_3D('',#11024,#8764,#8765);
#7197=AXIS2_PLACEMENT_3D('',#11025,#8766,#8767);
#7198=AXIS2_PLACEMENT_3D('',#11026,#8768,#8769);
#7199=AXIS2_PLACEMENT_3D('',#11027,#8770,#8771);
#7200=AXIS2_PLACEMENT_3D('',#11028,#8772,#8773);
#7201=AXIS2_PLACEMENT_3D('',#11029,#8774,#8775);
#7202=AXIS2_PLACEMENT_3D('',#11030,#8776,#8777);
#7203=AXIS2_PLACEMENT_3D('',#11031,#8778,#8779);
#7204=AXIS2_PLACEMENT_3D('',#11032,#8780,#8781);
#7205=AXIS2_PLACEMENT_3D('',#11033,#8782,#8783);
#7206=AXIS2_PLACEMENT_3D('',#11034,#8784,#8785);
#7207=AXIS2_PLACEMENT_3D('',#11035,#8786,#8787);
#7208=AXIS2_PLACEMENT_3D('',#11036,#8788,#8789);
#7209=AXIS2_PLACEMENT_3D('',#11037,#8790,#8791);
#7210=AXIS2_PLACEMENT_3D('',#11038,#8792,#8793);
#7211=AXIS2_PLACEMENT_3D('',#11039,#8794,#8795);
#7212=AXIS2_PLACEMENT_3D('',#11040,#8796,#8797);
#7213=AXIS2_PLACEMENT_3D('',#11041,#8798,#8799);
#7214=AXIS2_PLACEMENT_3D('',#11042,#8800,#8801);
#7215=AXIS2_PLACEMENT_3D('',#11043,#8802,#8803);
#7216=AXIS2_PLACEMENT_3D('',#11044,#8804,#8805);
#7217=AXIS2_PLACEMENT_3D('',#11045,#8806,#8807);
#7218=AXIS2_PLACEMENT_3D('',#11046,#8808,#8809);
#7219=AXIS2_PLACEMENT_3D('',#11047,#8810,#8811);
#7220=AXIS2_PLACEMENT_3D('',#11048,#8812,#8813);
#7221=AXIS2_PLACEMENT_3D('',#11049,#8814,#8815);
#7222=AXIS2_PLACEMENT_3D('',#11050,#8816,#8817);
#7223=AXIS2_PLACEMENT_3D('',#11051,#8818,#8819);
#7224=AXIS2_PLACEMENT_3D('',#11052,#8820,#8821);
#7225=AXIS2_PLACEMENT_3D('',#11053,#8822,#8823);
#7226=AXIS2_PLACEMENT_3D('',#11054,#8824,#8825);
#7227=AXIS2_PLACEMENT_3D('',#11055,#8826,#8827);
#7228=AXIS2_PLACEMENT_3D('',#11056,#8828,#8829);
#7229=AXIS2_PLACEMENT_3D('',#11057,#8830,#8831);
#7230=AXIS2_PLACEMENT_3D('',#11058,#8832,#8833);
#7231=AXIS2_PLACEMENT_3D('',#11059,#8834,#8835);
#7232=AXIS2_PLACEMENT_3D('',#11060,#8836,#8837);
#7233=AXIS2_PLACEMENT_3D('',#11061,#8838,#8839);
#7234=AXIS2_PLACEMENT_3D('',#11070,#8844,#8845);
#7235=AXIS2_PLACEMENT_3D('',#11072,#8846,#8847);
#7236=AXIS2_PLACEMENT_3D('',#11076,#8850,#8851);
#7237=AXIS2_PLACEMENT_3D('',#11082,#8855,#8856);
#7238=AXIS2_PLACEMENT_3D('',#11084,#8858,#8859);
#7239=AXIS2_PLACEMENT_3D('',#11085,#8860,#8861);
#7240=AXIS2_PLACEMENT_3D('',#11086,#8862,#8863);
#7241=AXIS2_PLACEMENT_3D('',#11088,#8864,#8865);
#7242=AXIS2_PLACEMENT_3D('',#11090,#8866,#8867);
#7243=AXIS2_PLACEMENT_3D('',#11091,#8868,#8869);
#7244=AXIS2_PLACEMENT_3D('',#11093,#8870,#8871);
#7245=AXIS2_PLACEMENT_3D('',#11095,#8872,#8873);
#7246=AXIS2_PLACEMENT_3D('',#11096,#8874,#8875);
#7247=AXIS2_PLACEMENT_3D('',#11098,#8877,#8878);
#7248=AXIS2_PLACEMENT_3D('',#11101,#8880,#8881);
#7249=AXIS2_PLACEMENT_3D('',#11102,#8882,#8883);
#7250=AXIS2_PLACEMENT_3D('',#11104,#8884,#8885);
#7251=AXIS2_PLACEMENT_3D('',#11106,#8887,#8888);
#7252=AXIS2_PLACEMENT_3D('',#11107,#8889,#8890);
#7253=AXIS2_PLACEMENT_3D('',#11108,#8891,#8892);
#7254=AXIS2_PLACEMENT_3D('',#11109,#8893,#8894);
#7255=AXIS2_PLACEMENT_3D('',#11111,#8895,#8896);
#7256=AXIS2_PLACEMENT_3D('',#11114,#8898,#8899);
#7257=AXIS2_PLACEMENT_3D('',#11115,#8900,#8901);
#7258=AXIS2_PLACEMENT_3D('',#11117,#8902,#8903);
#7259=AXIS2_PLACEMENT_3D('',#11120,#8905,#8906);
#7260=AXIS2_PLACEMENT_3D('',#11121,#8907,#8908);
#7261=AXIS2_PLACEMENT_3D('',#11122,#8909,#8910);
#7262=AXIS2_PLACEMENT_3D('',#11123,#8911,#8912);
#7263=AXIS2_PLACEMENT_3D('',#11124,#8913,#8914);
#7264=AXIS2_PLACEMENT_3D('',#11126,#8915,#8916);
#7265=AXIS2_PLACEMENT_3D('',#11129,#8918,#8919);
#7266=AXIS2_PLACEMENT_3D('',#11130,#8920,#8921);
#7267=AXIS2_PLACEMENT_3D('',#11132,#8922,#8923);
#7268=AXIS2_PLACEMENT_3D('',#11135,#8925,#8926);
#7269=AXIS2_PLACEMENT_3D('',#11136,#8927,#8928);
#7270=AXIS2_PLACEMENT_3D('',#11137,#8929,#8930);
#7271=AXIS2_PLACEMENT_3D('',#11138,#8931,#8932);
#7272=AXIS2_PLACEMENT_3D('',#11139,#8933,#8934);
#7273=AXIS2_PLACEMENT_3D('',#11141,#8935,#8936);
#7274=AXIS2_PLACEMENT_3D('',#11144,#8938,#8939);
#7275=AXIS2_PLACEMENT_3D('',#11145,#8940,#8941);
#7276=AXIS2_PLACEMENT_3D('',#11154,#8946,#8947);
#7277=AXIS2_PLACEMENT_3D('',#11160,#8951,#8952);
#7278=AXIS2_PLACEMENT_3D('',#11166,#8956,#8957);
#7279=AXIS2_PLACEMENT_3D('',#11172,#8961,#8962);
#7280=AXIS2_PLACEMENT_3D('',#11178,#8966,#8967);
#7281=AXIS2_PLACEMENT_3D('',#11181,#8970,#8971);
#7282=AXIS2_PLACEMENT_3D('',#11182,#8972,#8973);
#7283=AXIS2_PLACEMENT_3D('',#11183,#8974,#8975);
#7284=AXIS2_PLACEMENT_3D('',#11184,#8976,#8977);
#7285=AXIS2_PLACEMENT_3D('',#11186,#8978,#8979);
#7286=AXIS2_PLACEMENT_3D('',#11189,#8981,#8982);
#7287=AXIS2_PLACEMENT_3D('',#11190,#8983,#8984);
#7288=AXIS2_PLACEMENT_3D('',#11199,#8989,#8990);
#7289=AXIS2_PLACEMENT_3D('',#11205,#8994,#8995);
#7290=AXIS2_PLACEMENT_3D('',#11211,#8999,#9000);
#7291=AXIS2_PLACEMENT_3D('',#11217,#9004,#9005);
#7292=AXIS2_PLACEMENT_3D('',#11223,#9009,#9010);
#7293=AXIS2_PLACEMENT_3D('',#11226,#9013,#9014);
#7294=AXIS2_PLACEMENT_3D('',#11227,#9015,#9016);
#7295=AXIS2_PLACEMENT_3D('',#11228,#9017,#9018);
#7296=AXIS2_PLACEMENT_3D('',#11229,#9019,#9020);
#7297=AXIS2_PLACEMENT_3D('',#11233,#9022,#9023);
#7298=AXIS2_PLACEMENT_3D('',#11234,#9024,#9025);
#7299=AXIS2_PLACEMENT_3D('',#11247,#9026,#9027);
#7300=AXIS2_PLACEMENT_3D('',#11288,#9029,#9030);
#7301=AXIS2_PLACEMENT_3D('',#11299,#9031,#9032);
#7302=AXIS2_PLACEMENT_3D('',#11301,#9034,#9035);
#7303=AXIS2_PLACEMENT_3D('',#11310,#9040,#9041);
#7304=AXIS2_PLACEMENT_3D('',#11316,#9045,#9046);
#7305=AXIS2_PLACEMENT_3D('',#11322,#9050,#9051);
#7306=AXIS2_PLACEMENT_3D('',#11324,#9052,#9053);
#7307=AXIS2_PLACEMENT_3D('',#11325,#9054,#9055);
#7308=AXIS2_PLACEMENT_3D('',#11326,#9056,#9057);
#7309=AXIS2_PLACEMENT_3D('',#11327,#9058,#9059);
#7310=AXIS2_PLACEMENT_3D('',#11328,#9060,#9061);
#7311=AXIS2_PLACEMENT_3D('',#11330,#9062,#9063);
#7312=AXIS2_PLACEMENT_3D('',#11333,#9065,#9066);
#7313=AXIS2_PLACEMENT_3D('',#11334,#9067,#9068);
#7314=AXIS2_PLACEMENT_3D('',#11336,#9069,#9070);
#7315=AXIS2_PLACEMENT_3D('',#11339,#9072,#9073);
#7316=AXIS2_PLACEMENT_3D('',#11340,#9074,#9075);
#7317=AXIS2_PLACEMENT_3D('',#11342,#9076,#9077);
#7318=AXIS2_PLACEMENT_3D('',#11345,#9079,#9080);
#7319=AXIS2_PLACEMENT_3D('',#11346,#9081,#9082);
#7320=AXIS2_PLACEMENT_3D('',#11348,#9083,#9084);
#7321=AXIS2_PLACEMENT_3D('',#11351,#9086,#9087);
#7322=AXIS2_PLACEMENT_3D('',#11352,#9088,#9089);
#7323=AXIS2_PLACEMENT_3D('',#11354,#9090,#9091);
#7324=AXIS2_PLACEMENT_3D('',#11356,#9092,#9093);
#7325=AXIS2_PLACEMENT_3D('',#11357,#9094,#9095);
#7326=AXIS2_PLACEMENT_3D('',#11359,#9096,#9097);
#7327=AXIS2_PLACEMENT_3D('',#11361,#9098,#9099);
#7328=AXIS2_PLACEMENT_3D('',#11362,#9100,#9101);
#7329=AXIS2_PLACEMENT_3D('',#11364,#9103,#9104);
#7330=AXIS2_PLACEMENT_3D('',#11367,#9106,#9107);
#7331=AXIS2_PLACEMENT_3D('',#11368,#9108,#9109);
#7332=AXIS2_PLACEMENT_3D('',#11370,#9111,#9112);
#7333=AXIS2_PLACEMENT_3D('',#11371,#9113,#9114);
#7334=AXIS2_PLACEMENT_3D('',#11372,#9115,#9116);
#7335=AXIS2_PLACEMENT_3D('',#11389,#9125,#9126);
#7336=AXIS2_PLACEMENT_3D('',#11395,#9130,#9131);
#7337=AXIS2_PLACEMENT_3D('',#11399,#9134,#9135);
#7338=AXIS2_PLACEMENT_3D('',#11403,#9138,#9139);
#7339=AXIS2_PLACEMENT_3D('',#11407,#9142,#9143);
#7340=AXIS2_PLACEMENT_3D('',#11415,#9148,#9149);
#7341=AXIS2_PLACEMENT_3D('',#11417,#9151,#9152);
#7342=AXIS2_PLACEMENT_3D('',#11419,#9154,#9155);
#7343=AXIS2_PLACEMENT_3D('',#11421,#9157,#9158);
#7344=AXIS2_PLACEMENT_3D('',#11422,#9159,#9160);
#7345=AXIS2_PLACEMENT_3D('',#11423,#9161,#9162);
#7346=AXIS2_PLACEMENT_3D('',#11432,#9167,#9168);
#7347=AXIS2_PLACEMENT_3D('',#11438,#9172,#9173);
#7348=AXIS2_PLACEMENT_3D('',#11444,#9177,#9178);
#7349=AXIS2_PLACEMENT_3D('',#11450,#9182,#9183);
#7350=AXIS2_PLACEMENT_3D('',#11456,#9187,#9188);
#7351=AXIS2_PLACEMENT_3D('',#11459,#9191,#9192);
#7352=AXIS2_PLACEMENT_3D('',#11460,#9193,#9194);
#7353=AXIS2_PLACEMENT_3D('',#11462,#9195,#9196);
#7354=AXIS2_PLACEMENT_3D('',#11463,#9197,#9198);
#7355=AXIS2_PLACEMENT_3D('',#11465,#9199,#9200);
#7356=AXIS2_PLACEMENT_3D('',#11467,#9202,#9203);
#7357=AXIS2_PLACEMENT_3D('',#11469,#9204,#9205);
#7358=AXIS2_PLACEMENT_3D('',#11471,#9207,#9208);
#7359=AXIS2_PLACEMENT_3D('',#11473,#9209,#9210);
#7360=AXIS2_PLACEMENT_3D('',#11475,#9212,#9213);
#7361=AXIS2_PLACEMENT_3D('',#11476,#9214,#9215);
#7362=AXIS2_PLACEMENT_3D('',#11477,#9216,#9217);
#7363=AXIS2_PLACEMENT_3D('',#11478,#9218,#9219);
#7364=AXIS2_PLACEMENT_3D('',#11479,#9220,#9221);
#7365=AXIS2_PLACEMENT_3D('',#11480,#9222,#9223);
#7366=AXIS2_PLACEMENT_3D('',#11481,#9224,#9225);
#7367=AXIS2_PLACEMENT_3D('',#11482,#9226,#9227);
#7368=AXIS2_PLACEMENT_3D('',#11483,#9228,#9229);
#7369=AXIS2_PLACEMENT_3D('',#11484,#9230,#9231);
#7370=AXIS2_PLACEMENT_3D('',#11485,#9232,#9233);
#7371=DIRECTION('axis',(0.,0.,1.));
#7372=DIRECTION('refdir',(1.,0.,0.));
#7373=DIRECTION('axis',(0.,0.,1.));
#7374=DIRECTION('refdir',(1.,0.,0.));
#7375=DIRECTION('axis',(0.,0.,1.));
#7376=DIRECTION('refdir',(1.,0.,0.));
#7377=DIRECTION('center_axis',(0.,0.,1.));
#7378=DIRECTION('ref_axis',(1.,0.,0.));
#7379=DIRECTION('center_axis',(0.,0.,1.));
#7380=DIRECTION('ref_axis',(1.,0.,0.));
#7381=DIRECTION('',(0.,0.,1.));
#7382=DIRECTION('center_axis',(0.,0.,-1.));
#7383=DIRECTION('ref_axis',(1.,0.,0.));
#7384=DIRECTION('center_axis',(0.,0.,1.));
#7385=DIRECTION('ref_axis',(1.,0.,0.));
#7386=DIRECTION('center_axis',(0.,0.,1.));
#7387=DIRECTION('ref_axis',(1.,0.,0.));
#7388=DIRECTION('',(0.,0.,1.));
#7389=DIRECTION('center_axis',(0.,0.,-1.));
#7390=DIRECTION('ref_axis',(1.,0.,0.));
#7391=DIRECTION('center_axis',(0.,0.,1.));
#7392=DIRECTION('ref_axis',(1.,0.,0.));
#7393=DIRECTION('center_axis',(0.,0.,1.));
#7394=DIRECTION('ref_axis',(1.,0.,0.));
#7395=DIRECTION('',(0.,0.,1.));
#7396=DIRECTION('center_axis',(0.,0.,-1.));
#7397=DIRECTION('ref_axis',(1.,0.,0.));
#7398=DIRECTION('center_axis',(0.,0.,1.));
#7399=DIRECTION('ref_axis',(1.,0.,0.));
#7400=DIRECTION('center_axis',(0.,0.,1.));
#7401=DIRECTION('ref_axis',(1.,0.,0.));
#7402=DIRECTION('',(0.,0.,1.));
#7403=DIRECTION('center_axis',(0.,0.,-1.));
#7404=DIRECTION('ref_axis',(1.,0.,0.));
#7405=DIRECTION('center_axis',(0.,0.,1.));
#7406=DIRECTION('ref_axis',(1.,0.,0.));
#7407=DIRECTION('center_axis',(0.,0.,1.));
#7408=DIRECTION('ref_axis',(1.,0.,0.));
#7409=DIRECTION('',(0.,0.,1.));
#7410=DIRECTION('center_axis',(0.,0.,-1.));
#7411=DIRECTION('ref_axis',(1.,0.,0.));
#7412=DIRECTION('center_axis',(0.,0.,1.));
#7413=DIRECTION('ref_axis',(1.,0.,0.));
#7414=DIRECTION('center_axis',(0.,0.,1.));
#7415=DIRECTION('ref_axis',(1.,0.,0.));
#7416=DIRECTION('',(0.,0.,1.));
#7417=DIRECTION('center_axis',(0.,0.,-1.));
#7418=DIRECTION('ref_axis',(1.,0.,0.));
#7419=DIRECTION('center_axis',(0.,0.,1.));
#7420=DIRECTION('ref_axis',(1.,0.,0.));
#7421=DIRECTION('center_axis',(0.,0.,1.));
#7422=DIRECTION('ref_axis',(1.,0.,0.));
#7423=DIRECTION('',(0.,0.,1.));
#7424=DIRECTION('center_axis',(0.,0.,-1.));
#7425=DIRECTION('ref_axis',(1.,0.,0.));
#7426=DIRECTION('center_axis',(0.,0.,1.));
#7427=DIRECTION('ref_axis',(1.,0.,0.));
#7428=DIRECTION('center_axis',(0.,0.,1.));
#7429=DIRECTION('ref_axis',(1.,0.,0.));
#7430=DIRECTION('',(0.,0.,1.));
#7431=DIRECTION('center_axis',(0.,0.,-1.));
#7432=DIRECTION('ref_axis',(1.,0.,0.));
#7433=DIRECTION('center_axis',(0.,0.,1.));
#7434=DIRECTION('ref_axis',(1.,0.,0.));
#7435=DIRECTION('center_axis',(0.,0.,1.));
#7436=DIRECTION('ref_axis',(1.,0.,0.));
#7437=DIRECTION('',(0.,0.,1.));
#7438=DIRECTION('center_axis',(0.,0.,-1.));
#7439=DIRECTION('ref_axis',(1.,0.,0.));
#7440=DIRECTION('center_axis',(0.,0.,1.));
#7441=DIRECTION('ref_axis',(1.,0.,0.));
#7442=DIRECTION('center_axis',(0.,0.,1.));
#7443=DIRECTION('ref_axis',(1.,0.,0.));
#7444=DIRECTION('',(0.,0.,1.));
#7445=DIRECTION('center_axis',(0.,0.,-1.));
#7446=DIRECTION('ref_axis',(1.,0.,0.));
#7447=DIRECTION('center_axis',(0.,0.,1.));
#7448=DIRECTION('ref_axis',(1.,0.,0.));
#7449=DIRECTION('center_axis',(0.,0.,1.));
#7450=DIRECTION('ref_axis',(1.,0.,0.));
#7451=DIRECTION('',(0.,0.,1.));
#7452=DIRECTION('center_axis',(0.,0.,-1.));
#7453=DIRECTION('ref_axis',(1.,0.,0.));
#7454=DIRECTION('center_axis',(0.,0.,1.));
#7455=DIRECTION('ref_axis',(1.,0.,0.));
#7456=DIRECTION('center_axis',(0.,0.,1.));
#7457=DIRECTION('ref_axis',(1.,0.,0.));
#7458=DIRECTION('',(0.,0.,1.));
#7459=DIRECTION('center_axis',(0.,0.,-1.));
#7460=DIRECTION('ref_axis',(1.,0.,0.));
#7461=DIRECTION('center_axis',(0.,1.,0.));
#7462=DIRECTION('ref_axis',(-1.,0.,0.));
#7463=DIRECTION('',(-1.,0.,0.));
#7464=DIRECTION('',(0.,0.,1.));
#7465=DIRECTION('',(-1.,0.,0.));
#7466=DIRECTION('',(0.,0.,1.));
#7467=DIRECTION('center_axis',(1.,0.,0.));
#7468=DIRECTION('ref_axis',(0.,1.,0.));
#7469=DIRECTION('',(0.,1.,0.));
#7470=DIRECTION('',(0.,1.,0.));
#7471=DIRECTION('',(0.,0.,1.));
#7472=DIRECTION('center_axis',(0.,-1.,0.));
#7473=DIRECTION('ref_axis',(1.,0.,0.));
#7474=DIRECTION('',(1.,0.,0.));
#7475=DIRECTION('',(1.,0.,0.));
#7476=DIRECTION('',(0.,0.,1.));
#7477=DIRECTION('center_axis',(-1.,0.,0.));
#7478=DIRECTION('ref_axis',(0.,-1.,0.));
#7479=DIRECTION('',(0.,-1.,0.));
#7480=DIRECTION('',(0.,-1.,0.));
#7481=DIRECTION('center_axis',(0.,0.,1.));
#7482=DIRECTION('ref_axis',(1.,0.,0.));
#7483=DIRECTION('center_axis',(0.,0.,1.));
#7484=DIRECTION('ref_axis',(1.,0.,0.));
#7485=DIRECTION('axis',(0.,0.,1.));
#7486=DIRECTION('refdir',(1.,0.,0.));
#7487=DIRECTION('center_axis',(0.,1.,0.));
#7488=DIRECTION('ref_axis',(-1.,0.,0.));
#7489=DIRECTION('',(-1.,0.,0.));
#7490=DIRECTION('',(0.,0.,1.));
#7491=DIRECTION('',(-1.,0.,0.));
#7492=DIRECTION('',(0.,0.,1.));
#7493=DIRECTION('center_axis',(1.,0.,0.));
#7494=DIRECTION('ref_axis',(0.,1.,0.));
#7495=DIRECTION('',(0.,1.,0.));
#7496=DIRECTION('',(0.,1.,0.));
#7497=DIRECTION('',(0.,0.,1.));
#7498=DIRECTION('center_axis',(0.,-1.,0.));
#7499=DIRECTION('ref_axis',(1.,0.,0.));
#7500=DIRECTION('',(1.,0.,0.));
#7501=DIRECTION('',(1.,0.,0.));
#7502=DIRECTION('',(0.,0.,1.));
#7503=DIRECTION('center_axis',(-1.,0.,0.));
#7504=DIRECTION('ref_axis',(0.,-1.,0.));
#7505=DIRECTION('',(0.,-1.,0.));
#7506=DIRECTION('',(0.,-1.,0.));
#7507=DIRECTION('center_axis',(0.,0.,1.));
#7508=DIRECTION('ref_axis',(1.,0.,0.));
#7509=DIRECTION('center_axis',(0.,0.,1.));
#7510=DIRECTION('ref_axis',(1.,0.,0.));
#7511=DIRECTION('axis',(0.,0.,1.));
#7512=DIRECTION('refdir',(1.,0.,0.));
#7513=DIRECTION('center_axis',(0.,1.,0.));
#7514=DIRECTION('ref_axis',(-1.,0.,0.));
#7515=DIRECTION('',(-1.,0.,0.));
#7516=DIRECTION('',(0.,0.,1.));
#7517=DIRECTION('',(-1.,0.,0.));
#7518=DIRECTION('',(0.,0.,1.));
#7519=DIRECTION('center_axis',(1.,0.,0.));
#7520=DIRECTION('ref_axis',(0.,1.,0.));
#7521=DIRECTION('',(0.,1.,0.));
#7522=DIRECTION('',(0.,1.,0.));
#7523=DIRECTION('',(0.,0.,1.));
#7524=DIRECTION('center_axis',(0.,-1.,0.));
#7525=DIRECTION('ref_axis',(1.,0.,0.));
#7526=DIRECTION('',(1.,0.,0.));
#7527=DIRECTION('',(1.,0.,0.));
#7528=DIRECTION('',(0.,0.,1.));
#7529=DIRECTION('center_axis',(-1.,0.,0.));
#7530=DIRECTION('ref_axis',(0.,-1.,0.));
#7531=DIRECTION('',(0.,-1.,0.));
#7532=DIRECTION('',(0.,-1.,0.));
#7533=DIRECTION('center_axis',(0.,0.,1.));
#7534=DIRECTION('ref_axis',(1.,0.,0.));
#7535=DIRECTION('center_axis',(0.,0.,1.));
#7536=DIRECTION('ref_axis',(1.,0.,0.));
#7537=DIRECTION('axis',(0.,0.,1.));
#7538=DIRECTION('refdir',(1.,0.,0.));
#7539=DIRECTION('center_axis',(0.,1.,0.));
#7540=DIRECTION('ref_axis',(-1.,0.,0.));
#7541=DIRECTION('',(-1.,0.,0.));
#7542=DIRECTION('',(0.,0.,1.));
#7543=DIRECTION('',(-1.,0.,0.));
#7544=DIRECTION('',(0.,0.,1.));
#7545=DIRECTION('center_axis',(1.,0.,0.));
#7546=DIRECTION('ref_axis',(0.,1.,0.));
#7547=DIRECTION('',(0.,1.,0.));
#7548=DIRECTION('',(0.,1.,0.));
#7549=DIRECTION('',(0.,0.,1.));
#7550=DIRECTION('center_axis',(0.,-1.,0.));
#7551=DIRECTION('ref_axis',(1.,0.,0.));
#7552=DIRECTION('',(1.,0.,0.));
#7553=DIRECTION('',(1.,0.,0.));
#7554=DIRECTION('',(0.,0.,1.));
#7555=DIRECTION('center_axis',(-1.,0.,0.));
#7556=DIRECTION('ref_axis',(0.,-1.,0.));
#7557=DIRECTION('',(0.,-1.,0.));
#7558=DIRECTION('',(0.,-1.,0.));
#7559=DIRECTION('center_axis',(0.,0.,1.));
#7560=DIRECTION('ref_axis',(1.,0.,0.));
#7561=DIRECTION('center_axis',(0.,0.,1.));
#7562=DIRECTION('ref_axis',(1.,0.,0.));
#7563=DIRECTION('axis',(0.,0.,1.));
#7564=DIRECTION('refdir',(1.,0.,0.));
#7565=DIRECTION('center_axis',(0.,1.,0.));
#7566=DIRECTION('ref_axis',(-1.,0.,0.));
#7567=DIRECTION('',(-1.,0.,0.));
#7568=DIRECTION('',(0.,0.,1.));
#7569=DIRECTION('',(-1.,0.,0.));
#7570=DIRECTION('',(0.,0.,1.));
#7571=DIRECTION('center_axis',(1.,0.,0.));
#7572=DIRECTION('ref_axis',(0.,1.,0.));
#7573=DIRECTION('',(0.,1.,0.));
#7574=DIRECTION('',(0.,1.,0.));
#7575=DIRECTION('',(0.,0.,1.));
#7576=DIRECTION('center_axis',(0.,-1.,0.));
#7577=DIRECTION('ref_axis',(1.,0.,0.));
#7578=DIRECTION('',(1.,0.,0.));
#7579=DIRECTION('',(1.,0.,0.));
#7580=DIRECTION('',(0.,0.,1.));
#7581=DIRECTION('center_axis',(-1.,0.,0.));
#7582=DIRECTION('ref_axis',(0.,-1.,0.));
#7583=DIRECTION('',(0.,-1.,0.));
#7584=DIRECTION('',(0.,-1.,0.));
#7585=DIRECTION('center_axis',(0.,0.,1.));
#7586=DIRECTION('ref_axis',(1.,0.,0.));
#7587=DIRECTION('center_axis',(0.,0.,1.));
#7588=DIRECTION('ref_axis',(1.,0.,0.));
#7589=DIRECTION('axis',(0.,0.,1.));
#7590=DIRECTION('refdir',(1.,0.,0.));
#7591=DIRECTION('center_axis',(0.,0.,1.));
#7592=DIRECTION('ref_axis',(1.,0.,0.));
#7593=DIRECTION('center_axis',(0.,0.,1.));
#7594=DIRECTION('ref_axis',(1.,0.,0.));
#7595=DIRECTION('',(0.,0.,1.));
#7596=DIRECTION('center_axis',(0.,0.,-1.));
#7597=DIRECTION('ref_axis',(1.,0.,0.));
#7598=DIRECTION('center_axis',(0.,0.,1.));
#7599=DIRECTION('ref_axis',(1.,0.,0.));
#7600=DIRECTION('center_axis',(0.,0.,1.));
#7601=DIRECTION('ref_axis',(1.,0.,0.));
#7602=DIRECTION('',(0.,0.,1.));
#7603=DIRECTION('center_axis',(0.,0.,-1.));
#7604=DIRECTION('ref_axis',(1.,0.,0.));
#7605=DIRECTION('center_axis',(0.,1.,0.));
#7606=DIRECTION('ref_axis',(1.,0.,0.));
#7607=DIRECTION('center_axis',(0.,1.,0.));
#7608=DIRECTION('ref_axis',(1.,0.,0.));
#7609=DIRECTION('',(0.,1.,0.));
#7610=DIRECTION('center_axis',(0.,-1.,0.));
#7611=DIRECTION('ref_axis',(1.,0.,0.));
#7612=DIRECTION('center_axis',(0.,1.,0.));
#7613=DIRECTION('ref_axis',(1.,0.,0.));
#7614=DIRECTION('center_axis',(0.,1.,0.));
#7615=DIRECTION('ref_axis',(1.,0.,0.));
#7616=DIRECTION('',(0.,1.,0.));
#7617=DIRECTION('center_axis',(0.,-1.,0.));
#7618=DIRECTION('ref_axis',(1.,0.,0.));
#7619=DIRECTION('center_axis',(0.,1.,0.));
#7620=DIRECTION('ref_axis',(1.,0.,0.));
#7621=DIRECTION('center_axis',(0.,1.,0.));
#7622=DIRECTION('ref_axis',(1.,0.,0.));
#7623=DIRECTION('',(0.,1.,0.));
#7624=DIRECTION('center_axis',(0.,-1.,0.));
#7625=DIRECTION('ref_axis',(1.,0.,0.));
#7626=DIRECTION('center_axis',(0.,1.,0.));
#7627=DIRECTION('ref_axis',(1.,0.,0.));
#7628=DIRECTION('center_axis',(0.,1.,0.));
#7629=DIRECTION('ref_axis',(1.,0.,0.));
#7630=DIRECTION('',(0.,1.,0.));
#7631=DIRECTION('center_axis',(0.,-1.,0.));
#7632=DIRECTION('ref_axis',(1.,0.,0.));
#7633=DIRECTION('center_axis',(0.,1.,0.));
#7634=DIRECTION('ref_axis',(1.,0.,0.));
#7635=DIRECTION('center_axis',(0.,1.,0.));
#7636=DIRECTION('ref_axis',(1.,0.,0.));
#7637=DIRECTION('',(0.,1.,0.));
#7638=DIRECTION('center_axis',(0.,-1.,0.));
#7639=DIRECTION('ref_axis',(1.,0.,0.));
#7640=DIRECTION('center_axis',(0.,0.,1.));
#7641=DIRECTION('ref_axis',(1.,0.,0.));
#7642=DIRECTION('',(1.,0.,0.));
#7643=DIRECTION('',(0.,1.,0.));
#7644=DIRECTION('',(-1.,0.,0.));
#7645=DIRECTION('',(0.,1.,0.));
#7646=DIRECTION('center_axis',(0.,1.,0.));
#7647=DIRECTION('ref_axis',(1.,0.,0.));
#7648=DIRECTION('',(0.,0.,-1.));
#7649=DIRECTION('',(1.,0.,0.));
#7650=DIRECTION('',(0.,0.,1.));
#7651=DIRECTION('center_axis',(0.,1.,0.));
#7652=DIRECTION('ref_axis',(-1.,0.,0.));
#7653=DIRECTION('',(0.,0.,1.));
#7654=DIRECTION('',(-1.,0.,0.));
#7655=DIRECTION('',(0.,0.,1.));
#7656=DIRECTION('',(-1.,0.,0.));
#7657=DIRECTION('center_axis',(-1.,0.,0.));
#7658=DIRECTION('ref_axis',(0.,-1.,0.));
#7659=DIRECTION('',(0.,0.,1.));
#7660=DIRECTION('',(0.,-1.,0.));
#7661=DIRECTION('',(0.,-1.,0.));
#7662=DIRECTION('center_axis',(1.,0.,0.));
#7663=DIRECTION('ref_axis',(0.,1.,0.));
#7664=DIRECTION('',(0.,1.,0.));
#7665=DIRECTION('',(0.,0.,1.));
#7666=DIRECTION('',(0.,1.,0.));
#7667=DIRECTION('center_axis',(0.,-1.,0.));
#7668=DIRECTION('ref_axis',(1.,0.,0.));
#7669=DIRECTION('',(1.,0.,0.));
#7670=DIRECTION('center_axis',(0.,0.,1.));
#7671=DIRECTION('ref_axis',(1.,0.,0.));
#7672=DIRECTION('center_axis',(0.,0.,1.));
#7673=DIRECTION('ref_axis',(1.,0.,0.));
#7674=DIRECTION('axis',(0.,0.,1.));
#7675=DIRECTION('refdir',(1.,0.,0.));
#7676=DIRECTION('center_axis',(0.,1.,0.));
#7677=DIRECTION('ref_axis',(1.,0.,0.));
#7678=DIRECTION('center_axis',(0.,-1.,0.));
#7679=DIRECTION('ref_axis',(1.,0.,0.));
#7680=DIRECTION('',(0.,-1.,0.));
#7681=DIRECTION('center_axis',(0.,-1.,0.));
#7682=DIRECTION('ref_axis',(1.,0.,0.));
#7683=DIRECTION('center_axis',(0.,1.,0.));
#7684=DIRECTION('ref_axis',(1.,0.,0.));
#7685=DIRECTION('center_axis',(0.,1.,0.));
#7686=DIRECTION('ref_axis',(1.,0.,0.));
#7687=DIRECTION('',(0.,-1.,0.));
#7688=DIRECTION('center_axis',(0.,1.,0.));
#7689=DIRECTION('ref_axis',(1.,0.,0.));
#7690=DIRECTION('center_axis',(0.,1.,0.));
#7691=DIRECTION('ref_axis',(1.,0.,0.));
#7692=DIRECTION('center_axis',(0.,1.,0.));
#7693=DIRECTION('ref_axis',(1.,0.,0.));
#7694=DIRECTION('axis',(0.,0.,1.));
#7695=DIRECTION('refdir',(1.,0.,0.));
#7696=DIRECTION('center_axis',(0.,1.,0.));
#7697=DIRECTION('ref_axis',(1.,0.,0.));
#7698=DIRECTION('center_axis',(0.,-1.,0.));
#7699=DIRECTION('ref_axis',(1.,0.,0.));
#7700=DIRECTION('',(0.,-1.,0.));
#7701=DIRECTION('center_axis',(0.,-1.,0.));
#7702=DIRECTION('ref_axis',(1.,0.,0.));
#7703=DIRECTION('center_axis',(0.,1.,0.));
#7704=DIRECTION('ref_axis',(1.,0.,0.));
#7705=DIRECTION('center_axis',(0.,1.,0.));
#7706=DIRECTION('ref_axis',(1.,0.,0.));
#7707=DIRECTION('',(0.,-1.,0.));
#7708=DIRECTION('center_axis',(0.,1.,0.));
#7709=DIRECTION('ref_axis',(1.,0.,0.));
#7710=DIRECTION('center_axis',(0.,1.,0.));
#7711=DIRECTION('ref_axis',(1.,0.,0.));
#7712=DIRECTION('center_axis',(0.,1.,0.));
#7713=DIRECTION('ref_axis',(1.,0.,0.));
#7714=DIRECTION('axis',(0.,0.,1.));
#7715=DIRECTION('refdir',(1.,0.,0.));
#7716=DIRECTION('center_axis',(0.,1.,0.));
#7717=DIRECTION('ref_axis',(1.,0.,0.));
#7718=DIRECTION('center_axis',(0.,-1.,0.));
#7719=DIRECTION('ref_axis',(1.,0.,0.));
#7720=DIRECTION('',(0.,-1.,0.));
#7721=DIRECTION('center_axis',(0.,-1.,0.));
#7722=DIRECTION('ref_axis',(1.,0.,0.));
#7723=DIRECTION('center_axis',(0.,1.,0.));
#7724=DIRECTION('ref_axis',(1.,0.,0.));
#7725=DIRECTION('center_axis',(0.,1.,0.));
#7726=DIRECTION('ref_axis',(1.,0.,0.));
#7727=DIRECTION('',(0.,-1.,0.));
#7728=DIRECTION('center_axis',(0.,1.,0.));
#7729=DIRECTION('ref_axis',(1.,0.,0.));
#7730=DIRECTION('center_axis',(0.,1.,0.));
#7731=DIRECTION('ref_axis',(1.,0.,0.));
#7732=DIRECTION('center_axis',(0.,1.,0.));
#7733=DIRECTION('ref_axis',(1.,0.,0.));
#7734=DIRECTION('axis',(0.,0.,1.));
#7735=DIRECTION('refdir',(1.,0.,0.));
#7736=DIRECTION('center_axis',(0.,1.,0.));
#7737=DIRECTION('ref_axis',(1.,0.,0.));
#7738=DIRECTION('center_axis',(0.,-1.,0.));
#7739=DIRECTION('ref_axis',(1.,0.,0.));
#7740=DIRECTION('',(0.,-1.,0.));
#7741=DIRECTION('center_axis',(0.,-1.,0.));
#7742=DIRECTION('ref_axis',(1.,0.,0.));
#7743=DIRECTION('center_axis',(0.,1.,0.));
#7744=DIRECTION('ref_axis',(1.,0.,0.));
#7745=DIRECTION('center_axis',(0.,1.,0.));
#7746=DIRECTION('ref_axis',(1.,0.,0.));
#7747=DIRECTION('',(0.,-1.,0.));
#7748=DIRECTION('center_axis',(0.,1.,0.));
#7749=DIRECTION('ref_axis',(1.,0.,0.));
#7750=DIRECTION('center_axis',(0.,1.,0.));
#7751=DIRECTION('ref_axis',(1.,0.,0.));
#7752=DIRECTION('center_axis',(0.,1.,0.));
#7753=DIRECTION('ref_axis',(1.,0.,0.));
#7754=DIRECTION('axis',(0.,0.,1.));
#7755=DIRECTION('refdir',(1.,0.,0.));
#7756=DIRECTION('center_axis',(0.,0.,1.));
#7757=DIRECTION('ref_axis',(1.,0.,0.));
#7758=DIRECTION('center_axis',(0.,0.,1.));
#7759=DIRECTION('ref_axis',(1.,0.,0.));
#7760=DIRECTION('',(0.,0.,1.));
#7761=DIRECTION('center_axis',(0.,0.,-1.));
#7762=DIRECTION('ref_axis',(1.,0.,0.));
#7763=DIRECTION('center_axis',(0.,0.,1.));
#7764=DIRECTION('ref_axis',(1.,0.,0.));
#7765=DIRECTION('center_axis',(0.,0.,1.));
#7766=DIRECTION('ref_axis',(1.,0.,0.));
#7767=DIRECTION('',(0.,0.,1.));
#7768=DIRECTION('center_axis',(0.,0.,-1.));
#7769=DIRECTION('ref_axis',(1.,0.,0.));
#7770=DIRECTION('center_axis',(0.,1.,0.));
#7771=DIRECTION('ref_axis',(1.,0.,0.));
#7772=DIRECTION('center_axis',(0.,1.,0.));
#7773=DIRECTION('ref_axis',(1.,0.,0.));
#7774=DIRECTION('',(0.,1.,0.));
#7775=DIRECTION('center_axis',(0.,-1.,0.));
#7776=DIRECTION('ref_axis',(1.,0.,0.));
#7777=DIRECTION('center_axis',(0.,1.,0.));
#7778=DIRECTION('ref_axis',(1.,0.,0.));
#7779=DIRECTION('center_axis',(0.,1.,0.));
#7780=DIRECTION('ref_axis',(1.,0.,0.));
#7781=DIRECTION('',(0.,1.,0.));
#7782=DIRECTION('center_axis',(0.,-1.,0.));
#7783=DIRECTION('ref_axis',(1.,0.,0.));
#7784=DIRECTION('center_axis',(0.,1.,0.));
#7785=DIRECTION('ref_axis',(1.,0.,0.));
#7786=DIRECTION('center_axis',(0.,1.,0.));
#7787=DIRECTION('ref_axis',(1.,0.,0.));
#7788=DIRECTION('',(0.,1.,0.));
#7789=DIRECTION('center_axis',(0.,-1.,0.));
#7790=DIRECTION('ref_axis',(1.,0.,0.));
#7791=DIRECTION('center_axis',(0.,1.,0.));
#7792=DIRECTION('ref_axis',(1.,0.,0.));
#7793=DIRECTION('center_axis',(0.,1.,0.));
#7794=DIRECTION('ref_axis',(1.,0.,0.));
#7795=DIRECTION('',(0.,1.,0.));
#7796=DIRECTION('center_axis',(0.,-1.,0.));
#7797=DIRECTION('ref_axis',(1.,0.,0.));
#7798=DIRECTION('center_axis',(0.,1.,0.));
#7799=DIRECTION('ref_axis',(1.,0.,0.));
#7800=DIRECTION('center_axis',(0.,1.,0.));
#7801=DIRECTION('ref_axis',(1.,0.,0.));
#7802=DIRECTION('',(0.,1.,0.));
#7803=DIRECTION('center_axis',(0.,-1.,0.));
#7804=DIRECTION('ref_axis',(1.,0.,0.));
#7805=DIRECTION('center_axis',(0.,0.,1.));
#7806=DIRECTION('ref_axis',(1.,0.,0.));
#7807=DIRECTION('',(1.,0.,0.));
#7808=DIRECTION('',(0.,1.,0.));
#7809=DIRECTION('',(-1.,0.,0.));
#7810=DIRECTION('',(0.,1.,0.));
#7811=DIRECTION('center_axis',(0.,1.,0.));
#7812=DIRECTION('ref_axis',(1.,0.,0.));
#7813=DIRECTION('',(0.,0.,-1.));
#7814=DIRECTION('',(1.,0.,0.));
#7815=DIRECTION('',(0.,0.,1.));
#7816=DIRECTION('center_axis',(0.,1.,0.));
#7817=DIRECTION('ref_axis',(-1.,0.,0.));
#7818=DIRECTION('',(0.,0.,1.));
#7819=DIRECTION('',(-1.,0.,0.));
#7820=DIRECTION('',(0.,0.,1.));
#7821=DIRECTION('',(-1.,0.,0.));
#7822=DIRECTION('center_axis',(-1.,0.,0.));
#7823=DIRECTION('ref_axis',(0.,-1.,0.));
#7824=DIRECTION('',(0.,0.,1.));
#7825=DIRECTION('',(0.,-1.,0.));
#7826=DIRECTION('',(0.,-1.,0.));
#7827=DIRECTION('center_axis',(1.,0.,0.));
#7828=DIRECTION('ref_axis',(0.,1.,0.));
#7829=DIRECTION('',(0.,1.,0.));
#7830=DIRECTION('',(0.,0.,1.));
#7831=DIRECTION('',(0.,1.,0.));
#7832=DIRECTION('center_axis',(0.,-1.,0.));
#7833=DIRECTION('ref_axis',(1.,0.,0.));
#7834=DIRECTION('',(1.,0.,0.));
#7835=DIRECTION('center_axis',(0.,0.,1.));
#7836=DIRECTION('ref_axis',(1.,0.,0.));
#7837=DIRECTION('center_axis',(0.,0.,1.));
#7838=DIRECTION('ref_axis',(1.,0.,0.));
#7839=DIRECTION('axis',(0.,0.,1.));
#7840=DIRECTION('refdir',(1.,0.,0.));
#7841=DIRECTION('center_axis',(0.,1.,0.));
#7842=DIRECTION('ref_axis',(1.,0.,0.));
#7843=DIRECTION('center_axis',(0.,-1.,0.));
#7844=DIRECTION('ref_axis',(1.,0.,0.));
#7845=DIRECTION('',(0.,-1.,0.));
#7846=DIRECTION('center_axis',(0.,-1.,0.));
#7847=DIRECTION('ref_axis',(1.,0.,0.));
#7848=DIRECTION('center_axis',(0.,1.,0.));
#7849=DIRECTION('ref_axis',(1.,0.,0.));
#7850=DIRECTION('center_axis',(0.,1.,0.));
#7851=DIRECTION('ref_axis',(1.,0.,0.));
#7852=DIRECTION('',(0.,-1.,0.));
#7853=DIRECTION('center_axis',(0.,1.,0.));
#7854=DIRECTION('ref_axis',(1.,0.,0.));
#7855=DIRECTION('center_axis',(0.,1.,0.));
#7856=DIRECTION('ref_axis',(1.,0.,0.));
#7857=DIRECTION('center_axis',(0.,1.,0.));
#7858=DIRECTION('ref_axis',(1.,0.,0.));
#7859=DIRECTION('axis',(0.,0.,1.));
#7860=DIRECTION('refdir',(1.,0.,0.));
#7861=DIRECTION('center_axis',(0.,1.,0.));
#7862=DIRECTION('ref_axis',(1.,0.,0.));
#7863=DIRECTION('center_axis',(0.,-1.,0.));
#7864=DIRECTION('ref_axis',(1.,0.,0.));
#7865=DIRECTION('',(0.,-1.,0.));
#7866=DIRECTION('center_axis',(0.,-1.,0.));
#7867=DIRECTION('ref_axis',(1.,0.,0.));
#7868=DIRECTION('center_axis',(0.,1.,0.));
#7869=DIRECTION('ref_axis',(1.,0.,0.));
#7870=DIRECTION('center_axis',(0.,1.,0.));
#7871=DIRECTION('ref_axis',(1.,0.,0.));
#7872=DIRECTION('',(0.,-1.,0.));
#7873=DIRECTION('center_axis',(0.,1.,0.));
#7874=DIRECTION('ref_axis',(1.,0.,0.));
#7875=DIRECTION('center_axis',(0.,1.,0.));
#7876=DIRECTION('ref_axis',(1.,0.,0.));
#7877=DIRECTION('center_axis',(0.,1.,0.));
#7878=DIRECTION('ref_axis',(1.,0.,0.));
#7879=DIRECTION('axis',(0.,0.,1.));
#7880=DIRECTION('refdir',(1.,0.,0.));
#7881=DIRECTION('center_axis',(0.,1.,0.));
#7882=DIRECTION('ref_axis',(1.,0.,0.));
#7883=DIRECTION('center_axis',(0.,-1.,0.));
#7884=DIRECTION('ref_axis',(1.,0.,0.));
#7885=DIRECTION('',(0.,-1.,0.));
#7886=DIRECTION('center_axis',(0.,-1.,0.));
#7887=DIRECTION('ref_axis',(1.,0.,0.));
#7888=DIRECTION('center_axis',(0.,1.,0.));
#7889=DIRECTION('ref_axis',(1.,0.,0.));
#7890=DIRECTION('center_axis',(0.,1.,0.));
#7891=DIRECTION('ref_axis',(1.,0.,0.));
#7892=DIRECTION('',(0.,-1.,0.));
#7893=DIRECTION('center_axis',(0.,1.,0.));
#7894=DIRECTION('ref_axis',(1.,0.,0.));
#7895=DIRECTION('center_axis',(0.,1.,0.));
#7896=DIRECTION('ref_axis',(1.,0.,0.));
#7897=DIRECTION('center_axis',(0.,1.,0.));
#7898=DIRECTION('ref_axis',(1.,0.,0.));
#7899=DIRECTION('axis',(0.,0.,1.));
#7900=DIRECTION('refdir',(1.,0.,0.));
#7901=DIRECTION('center_axis',(0.,1.,0.));
#7902=DIRECTION('ref_axis',(1.,0.,0.));
#7903=DIRECTION('center_axis',(0.,-1.,0.));
#7904=DIRECTION('ref_axis',(1.,0.,0.));
#7905=DIRECTION('',(0.,-1.,0.));
#7906=DIRECTION('center_axis',(0.,-1.,0.));
#7907=DIRECTION('ref_axis',(1.,0.,0.));
#7908=DIRECTION('center_axis',(0.,1.,0.));
#7909=DIRECTION('ref_axis',(1.,0.,0.));
#7910=DIRECTION('center_axis',(0.,1.,0.));
#7911=DIRECTION('ref_axis',(1.,0.,0.));
#7912=DIRECTION('',(0.,-1.,0.));
#7913=DIRECTION('center_axis',(0.,1.,0.));
#7914=DIRECTION('ref_axis',(1.,0.,0.));
#7915=DIRECTION('center_axis',(0.,1.,0.));
#7916=DIRECTION('ref_axis',(1.,0.,0.));
#7917=DIRECTION('center_axis',(0.,1.,0.));
#7918=DIRECTION('ref_axis',(1.,0.,0.));
#7919=DIRECTION('axis',(0.,0.,1.));
#7920=DIRECTION('refdir',(1.,0.,0.));
#7921=DIRECTION('center_axis',(0.,0.,-1.));
#7922=DIRECTION('ref_axis',(0.,1.,0.));
#7923=DIRECTION('',(0.,1.,0.));
#7924=DIRECTION('',(1.,0.,0.));
#7925=DIRECTION('',(0.,-1.,0.));
#7926=DIRECTION('',(1.,0.,0.));
#7927=DIRECTION('center_axis',(0.,1.,-8.88178419700125E-16));
#7928=DIRECTION('ref_axis',(0.,8.88178419700125E-16,1.));
#7929=DIRECTION('',(0.,8.88178419700125E-16,1.));
#7930=DIRECTION('',(1.,0.,0.));
#7931=DIRECTION('',(0.,-8.88178419700125E-16,-1.));
#7932=DIRECTION('center_axis',(0.,-7.40148683083439E-16,-1.));
#7933=DIRECTION('ref_axis',(0.,1.,-7.40148683083439E-16));
#7934=DIRECTION('',(0.,1.,-7.40148683083439E-16));
#7935=DIRECTION('',(1.,0.,0.));
#7936=DIRECTION('',(0.,-1.,7.40148683083439E-16));
#7937=DIRECTION('center_axis',(0.,-0.707106781186547,-0.707106781186548));
#7938=DIRECTION('ref_axis',(0.,0.707106781186548,-0.707106781186547));
#7939=DIRECTION('',(0.,0.707106781186548,-0.707106781186547));
#7940=DIRECTION('',(1.,0.,0.));
#7941=DIRECTION('',(0.,-0.707106781186548,0.707106781186547));
#7942=DIRECTION('center_axis',(0.,-1.,2.77555756156289E-16));
#7943=DIRECTION('ref_axis',(0.,-2.77555756156289E-16,-1.));
#7944=DIRECTION('',(0.,-2.77555756156289E-16,-1.));
#7945=DIRECTION('',(1.,0.,0.));
#7946=DIRECTION('',(0.,2.77555756156289E-16,1.));
#7947=DIRECTION('center_axis',(0.,-0.707106781186547,0.707106781186548));
#7948=DIRECTION('ref_axis',(0.,-0.707106781186548,-0.707106781186547));
#7949=DIRECTION('',(0.,-0.707106781186548,-0.707106781186547));
#7950=DIRECTION('',(1.,0.,0.));
#7951=DIRECTION('',(0.,0.707106781186548,0.707106781186547));
#7952=DIRECTION('center_axis',(0.,7.40148683083438E-16,1.));
#7953=DIRECTION('ref_axis',(0.,-1.,7.40148683083438E-16));
#7954=DIRECTION('',(0.,-1.,7.40148683083438E-16));
#7955=DIRECTION('',(1.,0.,0.));
#7956=DIRECTION('',(0.,1.,-7.40148683083438E-16));
#7957=DIRECTION('center_axis',(0.,1.,-4.44089209850063E-16));
#7958=DIRECTION('ref_axis',(0.,4.44089209850063E-16,1.));
#7959=DIRECTION('',(0.,4.44089209850063E-16,1.));
#7960=DIRECTION('',(1.,0.,0.));
#7961=DIRECTION('',(0.,-4.44089209850063E-16,-1.));
#7962=DIRECTION('center_axis',(0.,2.41352831440251E-16,1.));
#7963=DIRECTION('ref_axis',(0.,-1.,2.41352831440251E-16));
#7964=DIRECTION('',(0.,-1.,2.41352831440251E-16));
#7965=DIRECTION('',(-1.,0.,0.));
#7966=DIRECTION('',(0.,1.,-2.41352831440251E-16));
#7967=DIRECTION('center_axis',(0.,-1.,2.41352831440251E-16));
#7968=DIRECTION('ref_axis',(0.,-2.41352831440251E-16,-1.));
#7969=DIRECTION('',(0.,-2.41352831440251E-16,-1.));
#7970=DIRECTION('',(1.,0.,0.));
#7971=DIRECTION('',(0.,2.41352831440251E-16,1.));
#7972=DIRECTION('',(1.,0.,0.));
#7973=DIRECTION('center_axis',(0.,0.,-1.));
#7974=DIRECTION('ref_axis',(0.,1.,0.));
#7975=DIRECTION('',(0.,1.,0.));
#7976=DIRECTION('',(1.,0.,0.));
#7977=DIRECTION('',(0.,-1.,0.));
#7978=DIRECTION('center_axis',(0.,-1.,0.));
#7979=DIRECTION('ref_axis',(0.,0.,-1.));
#7980=DIRECTION('',(0.,0.,-1.));
#7981=DIRECTION('',(1.,0.,0.));
#7982=DIRECTION('',(0.,0.,1.));
#7983=DIRECTION('center_axis',(0.,-0.707106781186547,0.707106781186548));
#7984=DIRECTION('ref_axis',(0.,-0.707106781186548,-0.707106781186547));
#7985=DIRECTION('',(0.,-0.707106781186548,-0.707106781186547));
#7986=DIRECTION('',(1.,0.,0.));
#7987=DIRECTION('',(0.,0.707106781186548,0.707106781186547));
#7988=DIRECTION('center_axis',(0.,0.,1.));
#7989=DIRECTION('ref_axis',(0.,-1.,0.));
#7990=DIRECTION('',(0.,-1.,0.));
#7991=DIRECTION('',(1.,0.,0.));
#7992=DIRECTION('',(0.,1.,0.));
#7993=DIRECTION('center_axis',(0.,0.707106781186548,0.707106781186547));
#7994=DIRECTION('ref_axis',(0.,-0.707106781186547,0.707106781186548));
#7995=DIRECTION('',(0.,-0.707106781186547,0.707106781186548));
#7996=DIRECTION('',(1.,0.,0.));
#7997=DIRECTION('',(0.,0.707106781186547,-0.707106781186548));
#7998=DIRECTION('center_axis',(0.,1.,0.));
#7999=DIRECTION('ref_axis',(0.,0.,1.));
#8000=DIRECTION('',(0.,0.,1.));
#8001=DIRECTION('',(1.,0.,0.));
#8002=DIRECTION('',(0.,0.,-1.));
#8003=DIRECTION('center_axis',(0.,0.,-1.));
#8004=DIRECTION('ref_axis',(0.,1.,0.));
#8005=DIRECTION('',(0.,1.,0.));
#8006=DIRECTION('',(1.,0.,0.));
#8007=DIRECTION('',(0.,-1.,0.));
#8008=DIRECTION('center_axis',(0.,1.,-2.41352831440251E-16));
#8009=DIRECTION('ref_axis',(0.,2.41352831440251E-16,1.));
#8010=DIRECTION('',(0.,2.41352831440251E-16,1.));
#8011=DIRECTION('',(-1.,0.,0.));
#8012=DIRECTION('',(0.,-2.41352831440251E-16,-1.));
#8013=DIRECTION('center_axis',(0.,0.,1.));
#8014=DIRECTION('ref_axis',(0.,-1.,0.));
#8015=DIRECTION('',(0.,-1.,0.));
#8016=DIRECTION('',(1.,0.,0.));
#8017=DIRECTION('',(0.,1.,0.));
#8018=DIRECTION('',(1.,0.,0.));
#8019=DIRECTION('center_axis',(0.,-1.,0.));
#8020=DIRECTION('ref_axis',(0.,0.,-1.));
#8021=DIRECTION('',(0.,0.,-1.));
#8022=DIRECTION('',(1.,0.,0.));
#8023=DIRECTION('',(0.,0.,1.));
#8024=DIRECTION('center_axis',(0.,0.,1.));
#8025=DIRECTION('ref_axis',(0.,-1.,0.));
#8026=DIRECTION('',(0.,-1.,0.));
#8027=DIRECTION('',(1.,0.,0.));
#8028=DIRECTION('',(0.,1.,0.));
#8029=DIRECTION('center_axis',(0.,0.707106781186548,0.707106781186548));
#8030=DIRECTION('ref_axis',(0.,-0.707106781186548,0.707106781186548));
#8031=DIRECTION('',(0.,-0.707106781186548,0.707106781186548));
#8032=DIRECTION('',(1.,0.,0.));
#8033=DIRECTION('',(0.,0.707106781186548,-0.707106781186548));
#8034=DIRECTION('center_axis',(0.,1.,0.));
#8035=DIRECTION('ref_axis',(0.,0.,1.));
#8036=DIRECTION('',(0.,0.,1.));
#8037=DIRECTION('',(1.,0.,0.));
#8038=DIRECTION('',(0.,0.,-1.));
#8039=DIRECTION('center_axis',(0.,0.707106781186548,-0.707106781186547));
#8040=DIRECTION('ref_axis',(0.,0.707106781186547,0.707106781186548));
#8041=DIRECTION('',(0.,0.707106781186547,0.707106781186548));
#8042=DIRECTION('',(1.,0.,0.));
#8043=DIRECTION('',(0.,-0.707106781186547,-0.707106781186548));
#8044=DIRECTION('center_axis',(0.,-7.40148683083438E-16,-1.));
#8045=DIRECTION('ref_axis',(0.,1.,-7.40148683083438E-16));
#8046=DIRECTION('',(0.,1.,-7.40148683083438E-16));
#8047=DIRECTION('',(1.,0.,0.));
#8048=DIRECTION('',(0.,-1.,7.40148683083438E-16));
#8049=DIRECTION('center_axis',(0.,-1.,0.));
#8050=DIRECTION('ref_axis',(0.,0.,-1.));
#8051=DIRECTION('',(0.,0.,-1.));
#8052=DIRECTION('',(1.,0.,0.));
#8053=DIRECTION('',(0.,0.,1.));
#8054=DIRECTION('center_axis',(0.,0.,-1.));
#8055=DIRECTION('ref_axis',(0.,1.,0.));
#8056=DIRECTION('',(0.,1.,0.));
#8057=DIRECTION('',(-1.,0.,0.));
#8058=DIRECTION('',(0.,-1.,0.));
#8059=DIRECTION('center_axis',(0.,1.,0.));
#8060=DIRECTION('ref_axis',(0.,0.,1.));
#8061=DIRECTION('',(0.,0.,1.));
#8062=DIRECTION('',(1.,0.,0.));
#8063=DIRECTION('',(0.,0.,-1.));
#8064=DIRECTION('',(1.,0.,0.));
#8065=DIRECTION('center_axis',(0.,0.,1.));
#8066=DIRECTION('ref_axis',(0.,-1.,0.));
#8067=DIRECTION('',(0.,-1.,0.));
#8068=DIRECTION('',(1.,0.,0.));
#8069=DIRECTION('',(0.,1.,0.));
#8070=DIRECTION('center_axis',(0.,1.,0.));
#8071=DIRECTION('ref_axis',(0.,0.,1.));
#8072=DIRECTION('',(0.,0.,1.));
#8073=DIRECTION('',(1.,0.,0.));
#8074=DIRECTION('',(0.,0.,-1.));
#8075=DIRECTION('center_axis',(0.,0.707106781186547,-0.707106781186548));
#8076=DIRECTION('ref_axis',(0.,0.707106781186548,0.707106781186547));
#8077=DIRECTION('',(0.,0.707106781186548,0.707106781186547));
#8078=DIRECTION('',(1.,0.,0.));
#8079=DIRECTION('',(0.,-0.707106781186548,-0.707106781186547));
#8080=DIRECTION('center_axis',(0.,0.,-1.));
#8081=DIRECTION('ref_axis',(0.,1.,0.));
#8082=DIRECTION('',(0.,1.,0.));
#8083=DIRECTION('',(1.,0.,0.));
#8084=DIRECTION('',(0.,-1.,0.));
#8085=DIRECTION('center_axis',(0.,-0.707106781186547,-0.707106781186548));
#8086=DIRECTION('ref_axis',(0.,0.707106781186548,-0.707106781186547));
#8087=DIRECTION('',(0.,0.707106781186548,-0.707106781186547));
#8088=DIRECTION('',(1.,0.,0.));
#8089=DIRECTION('',(0.,-0.707106781186548,0.707106781186547));
#8090=DIRECTION('center_axis',(0.,-1.,0.));
#8091=DIRECTION('ref_axis',(0.,0.,-1.));
#8092=DIRECTION('',(0.,0.,-1.));
#8093=DIRECTION('',(1.,0.,0.));
#8094=DIRECTION('',(0.,0.,1.));
#8095=DIRECTION('center_axis',(0.,0.,1.));
#8096=DIRECTION('ref_axis',(0.,-1.,0.));
#8097=DIRECTION('',(0.,-1.,0.));
#8098=DIRECTION('',(1.,0.,0.));
#8099=DIRECTION('',(0.,1.,0.));
#8100=DIRECTION('center_axis',(0.,-1.,0.));
#8101=DIRECTION('ref_axis',(0.,0.,-1.));
#8102=DIRECTION('',(0.,0.,-1.));
#8103=DIRECTION('',(-1.,0.,0.));
#8104=DIRECTION('',(0.,0.,1.));
#8105=DIRECTION('center_axis',(1.,0.,0.));
#8106=DIRECTION('ref_axis',(0.,0.,-1.));
#8107=DIRECTION('center_axis',(1.,0.,0.));
#8108=DIRECTION('ref_axis',(0.,0.,-1.));
#8109=DIRECTION('',(1.,0.,0.));
#8110=DIRECTION('center_axis',(-1.,0.,0.));
#8111=DIRECTION('ref_axis',(0.,0.,-1.));
#8112=DIRECTION('center_axis',(0.,1.,0.));
#8113=DIRECTION('ref_axis',(0.,0.,1.));
#8114=DIRECTION('',(0.,0.,1.));
#8115=DIRECTION('',(1.,0.,0.));
#8116=DIRECTION('',(0.,0.,1.));
#8117=DIRECTION('center_axis',(0.,1.,0.));
#8118=DIRECTION('ref_axis',(0.,0.,1.));
#8119=DIRECTION('',(0.,0.,1.));
#8120=DIRECTION('',(1.,0.,0.));
#8121=DIRECTION('',(0.,0.,1.));
#8122=DIRECTION('center_axis',(0.,0.,-1.));
#8123=DIRECTION('ref_axis',(0.,1.,0.));
#8124=DIRECTION('',(0.,1.,0.));
#8125=DIRECTION('',(0.,1.,0.));
#8126=DIRECTION('center_axis',(0.,0.,-1.));
#8127=DIRECTION('ref_axis',(0.,1.,0.));
#8128=DIRECTION('',(0.,1.,0.));
#8129=DIRECTION('',(1.,0.,0.));
#8130=DIRECTION('',(0.,1.,0.));
#8131=DIRECTION('center_axis',(0.,-1.,0.));
#8132=DIRECTION('ref_axis',(0.,0.,-1.));
#8133=DIRECTION('',(0.,0.,-1.));
#8134=DIRECTION('',(0.,0.,-1.));
#8135=DIRECTION('center_axis',(0.,-1.,0.));
#8136=DIRECTION('ref_axis',(0.,0.,-1.));
#8137=DIRECTION('',(0.,0.,-1.));
#8138=DIRECTION('',(1.,0.,0.));
#8139=DIRECTION('',(0.,0.,-1.));
#8140=DIRECTION('center_axis',(0.,0.,1.));
#8141=DIRECTION('ref_axis',(0.,-1.,0.));
#8142=DIRECTION('',(0.,-1.,0.));
#8143=DIRECTION('',(0.,-1.,0.));
#8144=DIRECTION('center_axis',(0.,0.,1.));
#8145=DIRECTION('ref_axis',(0.,-1.,0.));
#8146=DIRECTION('',(0.,-1.,0.));
#8147=DIRECTION('',(0.,-1.,0.));
#8148=DIRECTION('center_axis',(1.,0.,0.));
#8149=DIRECTION('ref_axis',(0.,0.,-1.));
#8150=DIRECTION('center_axis',(1.,0.,0.));
#8151=DIRECTION('ref_axis',(0.,0.,-1.));
#8152=DIRECTION('axis',(0.,0.,1.));
#8153=DIRECTION('refdir',(1.,0.,0.));
#8154=DIRECTION('center_axis',(0.,0.,1.));
#8155=DIRECTION('ref_axis',(1.,0.,0.));
#8156=DIRECTION('',(1.,0.,0.));
#8157=DIRECTION('',(0.,-1.,0.));
#8158=DIRECTION('',(-1.,0.,0.));
#8159=DIRECTION('',(0.,1.,0.));
#8160=DIRECTION('center_axis',(0.,1.,0.));
#8161=DIRECTION('ref_axis',(-1.,0.,0.));
#8162=DIRECTION('',(0.,0.,1.));
#8163=DIRECTION('',(-1.,0.,0.));
#8164=DIRECTION('',(0.,0.,1.));
#8165=DIRECTION('center_axis',(0.,0.,1.));
#8166=DIRECTION('ref_axis',(1.,0.,0.));
#8167=DIRECTION('',(0.,-1.,0.));
#8168=DIRECTION('',(1.,0.,0.));
#8169=DIRECTION('',(0.,1.,0.));
#8170=DIRECTION('center_axis',(0.,0.,-1.));
#8171=DIRECTION('ref_axis',(1.,0.,0.));
#8172=DIRECTION('center_axis',(-1.,0.,0.));
#8173=DIRECTION('ref_axis',(0.,-1.,0.));
#8174=DIRECTION('',(0.,0.,1.));
#8175=DIRECTION('',(0.,0.707106781186548,0.707106781186548));
#8176=DIRECTION('',(0.,-1.,0.));
#8177=DIRECTION('',(0.,0.707106781186548,-0.707106781186548));
#8178=DIRECTION('',(0.,0.,1.));
#8179=DIRECTION('',(0.,-1.,0.));
#8180=DIRECTION('',(0.,0.,1.));
#8181=DIRECTION('center_axis',(0.,-1.,0.));
#8182=DIRECTION('ref_axis',(1.,0.,0.));
#8183=DIRECTION('',(1.,0.,0.));
#8184=DIRECTION('',(0.,0.,1.));
#8185=DIRECTION('center_axis',(0.,0.,1.));
#8186=DIRECTION('ref_axis',(1.,0.,0.));
#8187=DIRECTION('',(-1.,0.,0.));
#8188=DIRECTION('',(0.,1.,0.));
#8189=DIRECTION('center_axis',(1.,0.,0.));
#8190=DIRECTION('ref_axis',(0.,1.,0.));
#8191=DIRECTION('',(0.,0.,1.));
#8192=DIRECTION('',(0.,-0.707106781186548,0.707106781186548));
#8193=DIRECTION('',(0.,1.,0.));
#8194=DIRECTION('',(0.,-0.707106781186548,-0.707106781186548));
#8195=DIRECTION('',(0.,0.,1.));
#8196=DIRECTION('center_axis',(0.,-1.,0.));
#8197=DIRECTION('ref_axis',(1.,0.,0.));
#8198=DIRECTION('',(-1.,0.,0.));
#8199=DIRECTION('center_axis',(0.,-0.707106781186548,-0.707106781186548));
#8200=DIRECTION('ref_axis',(-1.,0.,0.));
#8201=DIRECTION('',(1.,0.,0.));
#8202=DIRECTION('center_axis',(0.,0.707106781186548,0.707106781186548));
#8203=DIRECTION('ref_axis',(0.,0.707106781186547,-0.707106781186547));
#8204=DIRECTION('',(1.,0.,0.));
#8205=DIRECTION('center_axis',(0.,0.,1.));
#8206=DIRECTION('ref_axis',(1.,0.,0.));
#8207=DIRECTION('center_axis',(0.,0.,-1.));
#8208=DIRECTION('ref_axis',(1.,0.,0.));
#8209=DIRECTION('',(0.,0.,1.));
#8210=DIRECTION('center_axis',(0.,0.,-1.));
#8211=DIRECTION('ref_axis',(1.,0.,0.));
#8212=DIRECTION('center_axis',(0.,-0.707106781186548,0.707106781186548));
#8213=DIRECTION('ref_axis',(0.,0.707106781186547,0.707106781186547));
#8214=DIRECTION('center_axis',(0.,0.,-1.));
#8215=DIRECTION('ref_axis',(1.,0.,0.));
#8216=DIRECTION('center_axis',(0.,0.,1.));
#8217=DIRECTION('ref_axis',(1.,0.,0.));
#8218=DIRECTION('',(-1.,0.,0.));
#8219=DIRECTION('center_axis',(0.,0.,1.));
#8220=DIRECTION('ref_axis',(1.,0.,0.));
#8221=DIRECTION('',(-1.,0.,0.));
#8222=DIRECTION('center_axis',(0.,0.707106781186548,-0.707106781186548));
#8223=DIRECTION('ref_axis',(-1.,0.,0.));
#8224=DIRECTION('',(1.,0.,0.));
#8225=DIRECTION('center_axis',(0.,1.,0.));
#8226=DIRECTION('ref_axis',(-1.,0.,0.));
#8227=DIRECTION('axis',(0.,0.,1.));
#8228=DIRECTION('refdir',(1.,0.,0.));
#8229=DIRECTION('center_axis',(0.866025403784439,0.,-0.5));
#8230=DIRECTION('ref_axis',(0.5,0.,0.866025403784439));
#8231=DIRECTION('',(-0.5,0.,-0.866025403784439));
#8232=DIRECTION('',(0.,-1.,0.));
#8233=DIRECTION('',(0.5,0.,0.866025403784439));
#8234=DIRECTION('',(0.,-1.,0.));
#8235=DIRECTION('center_axis',(1.20185167898973E-16,0.,-1.));
#8236=DIRECTION('ref_axis',(1.,0.,1.20185167898973E-16));
#8237=DIRECTION('',(-1.,0.,-1.20185167898973E-16));
#8238=DIRECTION('',(0.,-1.,0.));
#8239=DIRECTION('',(1.,0.,1.20185167898973E-16));
#8240=DIRECTION('center_axis',(-0.866025403784439,0.,-0.5));
#8241=DIRECTION('ref_axis',(0.5,0.,-0.866025403784439));
#8242=DIRECTION('',(-0.5,0.,0.866025403784439));
#8243=DIRECTION('',(0.,-1.,0.));
#8244=DIRECTION('',(0.5,0.,-0.866025403784439));
#8245=DIRECTION('center_axis',(-0.866025403784439,0.,0.5));
#8246=DIRECTION('ref_axis',(-0.5,0.,-0.866025403784439));
#8247=DIRECTION('',(0.5,0.,0.866025403784439));
#8248=DIRECTION('',(0.,-1.,0.));
#8249=DIRECTION('',(-0.5,0.,-0.866025403784439));
#8250=DIRECTION('center_axis',(-2.40370335797945E-16,0.,1.));
#8251=DIRECTION('ref_axis',(-1.,0.,-2.40370335797945E-16));
#8252=DIRECTION('',(1.,0.,2.40370335797945E-16));
#8253=DIRECTION('',(0.,-1.,0.));
#8254=DIRECTION('',(-1.,0.,-2.40370335797945E-16));
#8255=DIRECTION('center_axis',(0.866025403784439,0.,0.5));
#8256=DIRECTION('ref_axis',(-0.5,0.,0.866025403784439));
#8257=DIRECTION('',(0.5,0.,-0.866025403784439));
#8258=DIRECTION('',(-0.5,0.,0.866025403784439));
#8259=DIRECTION('center_axis',(0.,1.,0.));
#8260=DIRECTION('ref_axis',(1.,0.,0.));
#8261=DIRECTION('center_axis',(0.,-1.,0.));
#8262=DIRECTION('ref_axis',(0.,0.,-1.));
#8263=DIRECTION('center_axis',(0.,1.,0.));
#8264=DIRECTION('ref_axis',(1.,0.,0.));
#8265=DIRECTION('center_axis',(0.,1.,0.));
#8266=DIRECTION('ref_axis',(1.,0.,0.));
#8267=DIRECTION('center_axis',(0.,1.,0.));
#8268=DIRECTION('ref_axis',(0.,0.,1.));
#8269=DIRECTION('center_axis',(0.,-1.,0.));
#8270=DIRECTION('ref_axis',(1.,0.,0.));
#8271=DIRECTION('center_axis',(0.,-1.,0.));
#8272=DIRECTION('ref_axis',(1.,0.,0.));
#8273=DIRECTION('center_axis',(0.,-1.,0.));
#8274=DIRECTION('ref_axis',(1.,0.,0.));
#8275=DIRECTION('',(0.707106781186548,0.707106781186547,8.65956056235493E-17));
#8276=DIRECTION('center_axis',(0.,-1.,0.));
#8277=DIRECTION('ref_axis',(1.,0.,0.));
#8278=DIRECTION('center_axis',(0.,-1.,0.));
#8279=DIRECTION('ref_axis',(1.,0.,0.));
#8280=DIRECTION('',(0.,1.,0.));
#8281=DIRECTION('center_axis',(0.,1.,0.));
#8282=DIRECTION('ref_axis',(1.,0.,0.));
#8283=DIRECTION('center_axis',(0.,-1.,0.));
#8284=DIRECTION('ref_axis',(1.,0.,0.));
#8285=DIRECTION('',(-0.707106781186547,0.707106781186548,-8.65956056235493E-17));
#8286=DIRECTION('center_axis',(0.,-1.,0.));
#8287=DIRECTION('ref_axis',(0.,0.,-1.));
#8288=DIRECTION('center_axis',(0.,-1.,0.));
#8289=DIRECTION('ref_axis',(1.,0.,0.));
#8290=DIRECTION('center_axis',(0.,1.,0.));
#8291=DIRECTION('ref_axis',(1.,0.,0.));
#8292=DIRECTION('center_axis',(0.,1.,0.));
#8293=DIRECTION('ref_axis',(1.,0.,0.));
#8294=DIRECTION('',(-0.447213595499958,0.894427190999916,-5.47678698264203E-17));
#8295=DIRECTION('center_axis',(0.,-1.,0.));
#8296=DIRECTION('ref_axis',(1.,0.,0.));
#8297=DIRECTION('',(0.,1.,0.));
#8298=DIRECTION('axis',(0.,0.,1.));
#8299=DIRECTION('refdir',(1.,0.,0.));
#8300=DIRECTION('center_axis',(0.866025403784439,0.,-0.5));
#8301=DIRECTION('ref_axis',(0.5,0.,0.866025403784439));
#8302=DIRECTION('',(-0.5,0.,-0.866025403784439));
#8303=DIRECTION('',(0.,-1.,0.));
#8304=DIRECTION('',(0.5,0.,0.866025403784439));
#8305=DIRECTION('',(0.,-1.,0.));
#8306=DIRECTION('center_axis',(1.92296268638356E-16,0.,-1.));
#8307=DIRECTION('ref_axis',(1.,0.,1.92296268638356E-16));
#8308=DIRECTION('',(-1.,0.,-1.92296268638356E-16));
#8309=DIRECTION('',(0.,-1.,0.));
#8310=DIRECTION('',(1.,0.,1.92296268638356E-16));
#8311=DIRECTION('center_axis',(-0.866025403784439,0.,-0.5));
#8312=DIRECTION('ref_axis',(0.5,0.,-0.866025403784439));
#8313=DIRECTION('',(-0.5,0.,0.866025403784438));
#8314=DIRECTION('',(0.,-1.,0.));
#8315=DIRECTION('',(0.5,0.,-0.866025403784438));
#8316=DIRECTION('center_axis',(-0.866025403784439,0.,0.5));
#8317=DIRECTION('ref_axis',(-0.5,0.,-0.866025403784439));
#8318=DIRECTION('',(0.5,0.,0.866025403784439));
#8319=DIRECTION('',(0.,-1.,0.));
#8320=DIRECTION('',(-0.5,0.,-0.866025403784439));
#8321=DIRECTION('center_axis',(-1.92296268638356E-16,0.,1.));
#8322=DIRECTION('ref_axis',(-1.,0.,-1.92296268638356E-16));
#8323=DIRECTION('',(1.,0.,1.92296268638356E-16));
#8324=DIRECTION('',(0.,-1.,0.));
#8325=DIRECTION('',(-1.,0.,-1.92296268638356E-16));
#8326=DIRECTION('center_axis',(0.866025403784439,0.,0.5));
#8327=DIRECTION('ref_axis',(-0.5,0.,0.866025403784439));
#8328=DIRECTION('',(0.5,0.,-0.866025403784439));
#8329=DIRECTION('',(-0.5,0.,0.866025403784439));
#8330=DIRECTION('center_axis',(0.,1.,0.));
#8331=DIRECTION('ref_axis',(1.,0.,0.));
#8332=DIRECTION('center_axis',(0.,-1.,0.));
#8333=DIRECTION('ref_axis',(0.,0.,-1.));
#8334=DIRECTION('center_axis',(0.,1.,0.));
#8335=DIRECTION('ref_axis',(1.,0.,0.));
#8336=DIRECTION('center_axis',(0.,1.,0.));
#8337=DIRECTION('ref_axis',(1.,0.,0.));
#8338=DIRECTION('center_axis',(0.,1.,0.));
#8339=DIRECTION('ref_axis',(0.,0.,1.));
#8340=DIRECTION('center_axis',(0.,-1.,0.));
#8341=DIRECTION('ref_axis',(1.,0.,0.));
#8342=DIRECTION('center_axis',(0.,-1.,0.));
#8343=DIRECTION('ref_axis',(1.,0.,0.));
#8344=DIRECTION('center_axis',(0.,-1.,0.));
#8345=DIRECTION('ref_axis',(1.,0.,0.));
#8346=DIRECTION('',(0.707106781186548,0.707106781186547,8.65956056235494E-17));
#8347=DIRECTION('center_axis',(0.,-1.,0.));
#8348=DIRECTION('ref_axis',(1.,0.,0.));
#8349=DIRECTION('center_axis',(0.,-1.,0.));
#8350=DIRECTION('ref_axis',(1.,0.,0.));
#8351=DIRECTION('',(0.,1.,0.));
#8352=DIRECTION('center_axis',(0.,1.,0.));
#8353=DIRECTION('ref_axis',(1.,0.,0.));
#8354=DIRECTION('center_axis',(0.,-1.,0.));
#8355=DIRECTION('ref_axis',(1.,0.,0.));
#8356=DIRECTION('',(-0.707106781186547,0.707106781186548,-8.65956056235493E-17));
#8357=DIRECTION('center_axis',(0.,-1.,0.));
#8358=DIRECTION('ref_axis',(0.,0.,-1.));
#8359=DIRECTION('center_axis',(0.,-1.,0.));
#8360=DIRECTION('ref_axis',(1.,0.,0.));
#8361=DIRECTION('center_axis',(0.,1.,0.));
#8362=DIRECTION('ref_axis',(1.,0.,0.));
#8363=DIRECTION('center_axis',(0.,1.,0.));
#8364=DIRECTION('ref_axis',(1.,0.,0.));
#8365=DIRECTION('',(-0.447213595499958,0.894427190999916,-5.47678698264203E-17));
#8366=DIRECTION('center_axis',(0.,-1.,0.));
#8367=DIRECTION('ref_axis',(1.,0.,0.));
#8368=DIRECTION('',(0.,1.,0.));
#8369=DIRECTION('axis',(0.,0.,1.));
#8370=DIRECTION('refdir',(1.,0.,0.));
#8371=DIRECTION('axis',(0.,0.,1.));
#8372=DIRECTION('refdir',(1.,0.,0.));
#8373=DIRECTION('center_axis',(0.,1.,0.));
#8374=DIRECTION('ref_axis',(1.,0.,0.));
#8375=DIRECTION('center_axis',(0.,1.,0.));
#8376=DIRECTION('ref_axis',(1.,0.,0.));
#8377=DIRECTION('',(0.,1.,0.));
#8378=DIRECTION('center_axis',(0.,-1.,0.));
#8379=DIRECTION('ref_axis',(1.,0.,0.));
#8380=DIRECTION('center_axis',(0.,1.,0.));
#8381=DIRECTION('ref_axis',(1.,0.,0.));
#8382=DIRECTION('center_axis',(0.,1.,0.));
#8383=DIRECTION('ref_axis',(1.,0.,0.));
#8384=DIRECTION('',(0.,1.,0.));
#8385=DIRECTION('center_axis',(0.,-1.,0.));
#8386=DIRECTION('ref_axis',(1.,0.,0.));
#8387=DIRECTION('center_axis',(6.12323399573677E-17,0.,1.));
#8388=DIRECTION('ref_axis',(1.,0.,0.));
#8389=DIRECTION('center_axis',(-1.22464679914735E-16,1.,0.));
#8390=DIRECTION('ref_axis',(-1.,-1.22464679914735E-16,0.));
#8391=DIRECTION('center_axis',(0.,1.,0.));
#8392=DIRECTION('ref_axis',(1.,0.,0.));
#8393=DIRECTION('center_axis',(0.,1.,0.));
#8394=DIRECTION('ref_axis',(1.,0.,0.));
#8395=DIRECTION('',(0.,-1.,0.));
#8396=DIRECTION('center_axis',(0.,-1.,0.));
#8397=DIRECTION('ref_axis',(1.,0.,0.));
#8398=DIRECTION('center_axis',(0.,1.,0.));
#8399=DIRECTION('ref_axis',(1.,0.,0.));
#8400=DIRECTION('center_axis',(0.,1.,0.));
#8401=DIRECTION('ref_axis',(1.,0.,0.));
#8402=DIRECTION('',(0.,-1.,0.));
#8403=DIRECTION('center_axis',(0.,-1.,0.));
#8404=DIRECTION('ref_axis',(1.,0.,0.));
#8405=DIRECTION('center_axis',(0.,1.,0.));
#8406=DIRECTION('ref_axis',(1.,0.,0.));
#8407=DIRECTION('center_axis',(0.,1.,0.));
#8408=DIRECTION('ref_axis',(1.,0.,0.));
#8409=DIRECTION('center_axis',(0.,1.,0.));
#8410=DIRECTION('ref_axis',(1.,0.,0.));
#8411=DIRECTION('center_axis',(0.,1.,0.));
#8412=DIRECTION('ref_axis',(1.,0.,0.));
#8413=DIRECTION('',(0.,1.,0.));
#8414=DIRECTION('center_axis',(0.,-1.,0.));
#8415=DIRECTION('ref_axis',(1.,0.,0.));
#8416=DIRECTION('center_axis',(0.,1.,0.));
#8417=DIRECTION('ref_axis',(1.,0.,0.));
#8418=DIRECTION('center_axis',(0.,1.,0.));
#8419=DIRECTION('ref_axis',(1.,0.,0.));
#8420=DIRECTION('',(0.,1.,0.));
#8421=DIRECTION('center_axis',(0.,-1.,0.));
#8422=DIRECTION('ref_axis',(1.,0.,0.));
#8423=DIRECTION('center_axis',(0.,1.,0.));
#8424=DIRECTION('ref_axis',(1.,0.,0.));
#8425=DIRECTION('center_axis',(0.,1.,0.));
#8426=DIRECTION('ref_axis',(1.,0.,0.));
#8427=DIRECTION('',(0.,1.,0.));
#8428=DIRECTION('center_axis',(0.,-1.,0.));
#8429=DIRECTION('ref_axis',(1.,0.,0.));
#8430=DIRECTION('center_axis',(0.,1.,0.));
#8431=DIRECTION('ref_axis',(1.,0.,0.));
#8432=DIRECTION('center_axis',(0.,1.,0.));
#8433=DIRECTION('ref_axis',(1.,0.,0.));
#8434=DIRECTION('',(0.,1.,0.));
#8435=DIRECTION('center_axis',(0.,-1.,0.));
#8436=DIRECTION('ref_axis',(1.,0.,0.));
#8437=DIRECTION('center_axis',(-1.,0.,0.));
#8438=DIRECTION('ref_axis',(0.,0.,1.));
#8439=DIRECTION('',(0.,0.,1.));
#8440=DIRECTION('',(0.,1.,0.));
#8441=DIRECTION('',(0.,0.,1.));
#8442=DIRECTION('',(0.,1.,0.));
#8443=DIRECTION('center_axis',(-0.707106781186548,0.,-0.707106781186548));
#8444=DIRECTION('ref_axis',(-0.707106781186548,0.,0.707106781186548));
#8445=DIRECTION('',(-0.707106781186548,0.,0.707106781186548));
#8446=DIRECTION('',(-0.707106781186548,0.,0.707106781186548));
#8447=DIRECTION('',(0.,1.,0.));
#8448=DIRECTION('center_axis',(0.,0.,-1.));
#8449=DIRECTION('ref_axis',(-1.,0.,0.));
#8450=DIRECTION('',(-1.,0.,0.));
#8451=DIRECTION('',(-1.,0.,0.));
#8452=DIRECTION('',(0.,1.,0.));
#8453=DIRECTION('center_axis',(0.707106781186548,0.,-0.707106781186548));
#8454=DIRECTION('ref_axis',(-0.707106781186548,0.,-0.707106781186548));
#8455=DIRECTION('',(-0.707106781186548,0.,-0.707106781186548));
#8456=DIRECTION('',(-0.707106781186548,0.,-0.707106781186548));
#8457=DIRECTION('',(0.,1.,0.));
#8458=DIRECTION('center_axis',(1.,0.,0.));
#8459=DIRECTION('ref_axis',(0.,0.,-1.));
#8460=DIRECTION('',(0.,0.,-1.));
#8461=DIRECTION('',(0.,0.,-1.));
#8462=DIRECTION('',(0.,1.,0.));
#8463=DIRECTION('center_axis',(0.707106781186548,0.,0.707106781186548));
#8464=DIRECTION('ref_axis',(0.707106781186548,0.,-0.707106781186548));
#8465=DIRECTION('',(0.707106781186548,0.,-0.707106781186548));
#8466=DIRECTION('',(0.707106781186548,0.,-0.707106781186548));
#8467=DIRECTION('',(0.,1.,0.));
#8468=DIRECTION('center_axis',(0.,0.,1.));
#8469=DIRECTION('ref_axis',(1.,0.,0.));
#8470=DIRECTION('',(1.,0.,0.));
#8471=DIRECTION('',(1.,0.,0.));
#8472=DIRECTION('',(0.,1.,0.));
#8473=DIRECTION('center_axis',(-0.707106781186548,0.,0.707106781186548));
#8474=DIRECTION('ref_axis',(0.707106781186548,0.,0.707106781186548));
#8475=DIRECTION('',(0.707106781186548,0.,0.707106781186548));
#8476=DIRECTION('',(0.707106781186548,0.,0.707106781186548));
#8477=DIRECTION('center_axis',(0.,1.,0.));
#8478=DIRECTION('ref_axis',(0.,0.,1.));
#8479=DIRECTION('center_axis',(0.,1.,0.));
#8480=DIRECTION('ref_axis',(1.,0.,0.));
#8481=DIRECTION('axis',(0.,0.,1.));
#8482=DIRECTION('refdir',(1.,0.,0.));
#8483=DIRECTION('center_axis',(0.,-1.,0.));
#8484=DIRECTION('ref_axis',(1.,0.,0.));
#8485=DIRECTION('center_axis',(0.,-1.,0.));
#8486=DIRECTION('ref_axis',(1.,0.,0.));
#8487=DIRECTION('',(0.,1.,0.));
#8488=DIRECTION('center_axis',(0.,-1.,0.));
#8489=DIRECTION('ref_axis',(1.,0.,0.));
#8490=DIRECTION('center_axis',(0.,1.,0.));
#8491=DIRECTION('ref_axis',(0.,0.,1.));
#8492=DIRECTION('center_axis',(0.,-1.,0.));
#8493=DIRECTION('ref_axis',(1.,0.,0.));
#8494=DIRECTION('center_axis',(6.12323399573677E-17,0.,1.));
#8495=DIRECTION('ref_axis',(1.,0.,0.));
#8496=DIRECTION('center_axis',(1.22464679914735E-16,-1.,0.));
#8497=DIRECTION('ref_axis',(-1.,-1.22464679914735E-16,0.));
#8498=DIRECTION('center_axis',(0.,-1.,0.));
#8499=DIRECTION('ref_axis',(1.,0.,0.));
#8500=DIRECTION('center_axis',(0.,-1.,0.));
#8501=DIRECTION('ref_axis',(0.,0.,-1.));
#8502=DIRECTION('center_axis',(-0.866025403784438,0.,-0.5));
#8503=DIRECTION('ref_axis',(-0.5,0.,0.866025403784438));
#8504=DIRECTION('',(-0.866025403784438,0.,-0.5));
#8505=DIRECTION('center_axis',(-0.866025403784438,0.,-0.5));
#8506=DIRECTION('ref_axis',(-0.5,0.,0.866025403784438));
#8507=DIRECTION('',(-0.866025403784438,0.,-0.5));
#8508=DIRECTION('center_axis',(0.,-1.,0.));
#8509=DIRECTION('ref_axis',(1.,0.,0.));
#8510=DIRECTION('center_axis',(0.,-1.,0.));
#8511=DIRECTION('ref_axis',(1.,0.,0.));
#8512=DIRECTION('',(0.,1.,0.));
#8513=DIRECTION('center_axis',(0.,-1.,0.));
#8514=DIRECTION('ref_axis',(1.,0.,0.));
#8515=DIRECTION('center_axis',(0.866025403784439,0.,-0.5));
#8516=DIRECTION('ref_axis',(-0.5,0.,-0.866025403784439));
#8517=DIRECTION('',(0.866025403784439,0.,-0.5));
#8518=DIRECTION('center_axis',(0.866025403784439,0.,-0.5));
#8519=DIRECTION('ref_axis',(-0.5,0.,-0.866025403784439));
#8520=DIRECTION('',(0.866025403784439,0.,-0.5));
#8521=DIRECTION('center_axis',(0.,0.,1.));
#8522=DIRECTION('ref_axis',(1.,0.,0.));
#8523=DIRECTION('',(0.,0.,1.));
#8524=DIRECTION('center_axis',(0.,0.,1.));
#8525=DIRECTION('ref_axis',(1.,0.,0.));
#8526=DIRECTION('',(0.,0.,1.));
#8527=DIRECTION('center_axis',(0.,1.,0.));
#8528=DIRECTION('ref_axis',(0.,0.,1.));
#8529=DIRECTION('center_axis',(0.,-1.,0.));
#8530=DIRECTION('ref_axis',(1.,0.,0.));
#8531=DIRECTION('center_axis',(0.,1.,0.));
#8532=DIRECTION('ref_axis',(0.,0.,1.));
#8533=DIRECTION('center_axis',(0.,-1.,0.));
#8534=DIRECTION('ref_axis',(1.,0.,0.));
#8535=DIRECTION('center_axis',(0.,-1.,0.));
#8536=DIRECTION('ref_axis',(1.,0.,0.));
#8537=DIRECTION('center_axis',(0.,-1.,0.));
#8538=DIRECTION('ref_axis',(1.,0.,0.));
#8539=DIRECTION('',(0.,1.,0.));
#8540=DIRECTION('center_axis',(0.,-1.,0.));
#8541=DIRECTION('ref_axis',(0.,0.,-1.));
#8542=DIRECTION('center_axis',(0.,-1.,0.));
#8543=DIRECTION('ref_axis',(1.,0.,0.));
#8544=DIRECTION('center_axis',(0.,-1.,0.));
#8545=DIRECTION('ref_axis',(1.,0.,0.));
#8546=DIRECTION('',(0.,1.,0.));
#8547=DIRECTION('',(0.,0.,1.));
#8548=DIRECTION('',(1.,0.,0.));
#8549=DIRECTION('',(0.,0.,1.));
#8550=DIRECTION('',(1.,0.,0.));
#8551=DIRECTION('axis',(0.,0.,1.));
#8552=DIRECTION('refdir',(1.,0.,0.));
#8553=DIRECTION('center_axis',(0.,1.,0.));
#8554=DIRECTION('ref_axis',(0.,0.,1.));
#8555=DIRECTION('center_axis',(0.,-1.,0.));
#8556=DIRECTION('ref_axis',(1.,0.,0.));
#8557=DIRECTION('center_axis',(0.,-1.,0.));
#8558=DIRECTION('ref_axis',(1.,0.,0.));
#8559=DIRECTION('center_axis',(0.,-1.,0.));
#8560=DIRECTION('ref_axis',(1.,0.,0.));
#8561=DIRECTION('',(0.707106781186548,0.707106781186547,8.65956056235493E-17));
#8562=DIRECTION('center_axis',(0.,-1.,0.));
#8563=DIRECTION('ref_axis',(1.,0.,0.));
#8564=DIRECTION('center_axis',(0.,-1.,0.));
#8565=DIRECTION('ref_axis',(1.,0.,0.));
#8566=DIRECTION('',(0.,1.,0.));
#8567=DIRECTION('center_axis',(0.,1.,0.));
#8568=DIRECTION('ref_axis',(1.,0.,0.));
#8569=DIRECTION('center_axis',(0.,-1.,0.));
#8570=DIRECTION('ref_axis',(1.,0.,0.));
#8571=DIRECTION('',(-0.707106781186548,0.707106781186547,-8.65956056235494E-17));
#8572=DIRECTION('center_axis',(0.,-1.,0.));
#8573=DIRECTION('ref_axis',(0.,0.,-1.));
#8574=DIRECTION('center_axis',(0.,-1.,0.));
#8575=DIRECTION('ref_axis',(1.,0.,0.));
#8576=DIRECTION('center_axis',(0.,1.,0.));
#8577=DIRECTION('ref_axis',(1.,0.,0.));
#8578=DIRECTION('center_axis',(0.,1.,0.));
#8579=DIRECTION('ref_axis',(1.,0.,0.));
#8580=DIRECTION('',(-0.447213595499958,0.894427190999916,-5.47678698264203E-17));
#8581=DIRECTION('center_axis',(0.,-1.,0.));
#8582=DIRECTION('ref_axis',(1.,0.,0.));
#8583=DIRECTION('center_axis',(0.,1.,0.));
#8584=DIRECTION('ref_axis',(1.,0.,0.));
#8585=DIRECTION('',(0.,1.,0.));
#8586=DIRECTION('center_axis',(0.,1.,0.));
#8587=DIRECTION('ref_axis',(1.,0.,0.));
#8588=DIRECTION('center_axis',(0.,-1.,0.));
#8589=DIRECTION('ref_axis',(1.,0.,0.));
#8590=DIRECTION('',(-0.707106781186547,0.707106781186548,-8.65956056235493E-17));
#8591=DIRECTION('center_axis',(0.,-1.,0.));
#8592=DIRECTION('ref_axis',(0.,0.,-1.));
#8593=DIRECTION('center_axis',(0.866025403784439,0.,-0.5));
#8594=DIRECTION('ref_axis',(0.5,0.,0.866025403784439));
#8595=DIRECTION('',(-0.5,0.,-0.866025403784439));
#8596=DIRECTION('',(0.,-1.,0.));
#8597=DIRECTION('',(0.5,0.,0.866025403784439));
#8598=DIRECTION('',(0.,-1.,0.));
#8599=DIRECTION('center_axis',(1.60246890531964E-16,0.,-1.));
#8600=DIRECTION('ref_axis',(1.,0.,1.60246890531964E-16));
#8601=DIRECTION('',(-1.,0.,-1.60246890531964E-16));
#8602=DIRECTION('',(0.,-1.,0.));
#8603=DIRECTION('',(1.,0.,1.60246890531964E-16));
#8604=DIRECTION('center_axis',(-0.866025403784439,0.,-0.5));
#8605=DIRECTION('ref_axis',(0.5,0.,-0.866025403784439));
#8606=DIRECTION('',(-0.5,0.,0.866025403784439));
#8607=DIRECTION('',(0.,-1.,0.));
#8608=DIRECTION('',(0.5,0.,-0.866025403784439));
#8609=DIRECTION('center_axis',(-0.866025403784439,0.,0.5));
#8610=DIRECTION('ref_axis',(-0.5,0.,-0.866025403784439));
#8611=DIRECTION('',(0.5,0.,0.866025403784439));
#8612=DIRECTION('',(0.,-1.,0.));
#8613=DIRECTION('',(-0.5,0.,-0.866025403784439));
#8614=DIRECTION('center_axis',(-1.60246890531964E-16,0.,1.));
#8615=DIRECTION('ref_axis',(-1.,0.,-1.60246890531964E-16));
#8616=DIRECTION('',(1.,0.,1.60246890531964E-16));
#8617=DIRECTION('',(0.,-1.,0.));
#8618=DIRECTION('',(-1.,0.,-1.60246890531964E-16));
#8619=DIRECTION('center_axis',(0.866025403784439,0.,0.5));
#8620=DIRECTION('ref_axis',(-0.5,0.,0.866025403784439));
#8621=DIRECTION('',(0.5,0.,-0.866025403784439));
#8622=DIRECTION('',(-0.5,0.,0.866025403784439));
#8623=DIRECTION('center_axis',(0.,1.,0.));
#8624=DIRECTION('ref_axis',(1.,0.,0.));
#8625=DIRECTION('center_axis',(0.,-1.,0.));
#8626=DIRECTION('ref_axis',(0.,0.,-1.));
#8627=DIRECTION('axis',(0.,0.,1.));
#8628=DIRECTION('refdir',(1.,0.,0.));
#8629=DIRECTION('center_axis',(0.,1.,0.));
#8630=DIRECTION('ref_axis',(1.,0.,0.));
#8631=DIRECTION('center_axis',(0.,-1.,0.));
#8632=DIRECTION('ref_axis',(1.,0.,0.));
#8633=DIRECTION('',(0.,-1.,0.));
#8634=DIRECTION('center_axis',(0.,-1.,0.));
#8635=DIRECTION('ref_axis',(1.,0.,0.));
#8636=DIRECTION('center_axis',(0.,1.,0.));
#8637=DIRECTION('ref_axis',(1.,0.,0.));
#8638=DIRECTION('center_axis',(0.,1.,0.));
#8639=DIRECTION('ref_axis',(1.,0.,0.));
#8640=DIRECTION('',(0.,-1.,0.));
#8641=DIRECTION('center_axis',(0.,1.,0.));
#8642=DIRECTION('ref_axis',(1.,0.,0.));
#8643=DIRECTION('center_axis',(0.,1.,0.));
#8644=DIRECTION('ref_axis',(1.,0.,0.));
#8645=DIRECTION('center_axis',(0.,1.,0.));
#8646=DIRECTION('ref_axis',(1.,0.,0.));
#8647=DIRECTION('axis',(0.,0.,1.));
#8648=DIRECTION('refdir',(1.,0.,0.));
#8649=DIRECTION('center_axis',(0.,1.,0.));
#8650=DIRECTION('ref_axis',(1.,0.,0.));
#8651=DIRECTION('',(0.866025403784439,-0.5,1.06057523872491E-16));
#8652=DIRECTION('center_axis',(0.,-1.,0.));
#8653=DIRECTION('ref_axis',(1.,0.,0.));
#8654=DIRECTION('center_axis',(0.,-1.,0.));
#8655=DIRECTION('ref_axis',(1.,0.,0.));
#8656=DIRECTION('center_axis',(0.,1.,0.));
#8657=DIRECTION('ref_axis',(1.,0.,0.));
#8658=DIRECTION('',(-0.866025403784439,-0.5,-1.06057523872491E-16));
#8659=DIRECTION('center_axis',(1.4792020664489E-16,0.,-1.));
#8660=DIRECTION('ref_axis',(-1.,0.,-1.4792020664489E-16));
#8661=DIRECTION('',(0.,1.,0.));
#8662=DIRECTION('',(0.,1.,0.));
#8663=DIRECTION('center_axis',(-0.866025403784439,0.,-0.5));
#8664=DIRECTION('ref_axis',(-0.5,0.,0.866025403784439));
#8665=DIRECTION('',(0.,1.,0.));
#8666=DIRECTION('center_axis',(-0.866025403784439,0.,0.5));
#8667=DIRECTION('ref_axis',(0.5,0.,0.866025403784439));
#8668=DIRECTION('',(0.,1.,0.));
#8669=DIRECTION('center_axis',(0.,1.,0.));
#8670=DIRECTION('ref_axis',(1.,0.,0.));
#8671=DIRECTION('center_axis',(0.,1.,0.));
#8672=DIRECTION('ref_axis',(1.,0.,0.));
#8673=DIRECTION('',(0.,-1.,0.));
#8674=DIRECTION('center_axis',(0.,1.,0.));
#8675=DIRECTION('ref_axis',(1.,0.,0.));
#8676=DIRECTION('center_axis',(-2.95840413289779E-16,0.,1.));
#8677=DIRECTION('ref_axis',(1.,0.,2.95840413289779E-16));
#8678=DIRECTION('',(0.,1.,0.));
#8679=DIRECTION('center_axis',(0.866025403784439,0.,-0.5));
#8680=DIRECTION('ref_axis',(-0.5,0.,-0.866025403784439));
#8681=DIRECTION('',(0.,1.,0.));
#8682=DIRECTION('center_axis',(0.866025403784439,0.,0.5));
#8683=DIRECTION('ref_axis',(0.5,0.,-0.866025403784439));
#8684=DIRECTION('center_axis',(0.,1.,0.));
#8685=DIRECTION('ref_axis',(1.,0.,0.));
#8686=DIRECTION('center_axis',(0.,1.,0.));
#8687=DIRECTION('ref_axis',(1.,0.,0.));
#8688=DIRECTION('',(0.,0.,1.));
#8689=DIRECTION('',(1.,0.,0.));
#8690=DIRECTION('',(0.,0.,1.));
#8691=DIRECTION('',(1.,0.,0.));
#8692=DIRECTION('',(0.,0.,1.));
#8693=DIRECTION('',(1.,0.,0.));
#8694=DIRECTION('',(0.,0.,1.));
#8695=DIRECTION('',(1.,0.,0.));
#8696=DIRECTION('',(0.,0.,1.));
#8697=DIRECTION('',(1.,0.,0.));
#8698=DIRECTION('',(0.,0.,1.));
#8699=DIRECTION('',(1.,0.,0.));
#8700=DIRECTION('',(0.,0.,1.));
#8701=DIRECTION('',(1.,0.,0.));
#8702=DIRECTION('',(0.,0.,1.));
#8703=DIRECTION('',(1.,0.,0.));
#8704=DIRECTION('',(0.,0.,1.));
#8705=DIRECTION('',(1.,0.,0.));
#8706=DIRECTION('',(0.,0.,1.));
#8707=DIRECTION('',(1.,0.,0.));
#8708=DIRECTION('',(0.,0.,1.));
#8709=DIRECTION('',(1.,0.,0.));
#8710=DIRECTION('',(0.,0.,1.));
#8711=DIRECTION('',(1.,0.,0.));
#8712=DIRECTION('',(0.,0.,1.));
#8713=DIRECTION('',(1.,0.,0.));
#8714=DIRECTION('',(0.,0.,1.));
#8715=DIRECTION('',(1.,0.,0.));
#8716=DIRECTION('',(0.,0.,1.));
#8717=DIRECTION('',(1.,0.,0.));
#8718=DIRECTION('',(0.,0.,1.));
#8719=DIRECTION('',(1.,0.,0.));
#8720=DIRECTION('',(0.,0.,1.));
#8721=DIRECTION('',(1.,0.,0.));
#8722=DIRECTION('',(0.,-1.,2.22044604925031E-16));
#8723=DIRECTION('',(1.,0.,0.));
#8724=DIRECTION('',(0.,0.,1.));
#8725=DIRECTION('',(1.,0.,0.));
#8726=DIRECTION('',(0.,-1.,2.22044604925031E-16));
#8727=DIRECTION('',(1.,0.,0.));
#8728=DIRECTION('',(0.,0.,1.));
#8729=DIRECTION('',(1.,0.,0.));
#8730=DIRECTION('',(0.,0.,1.));
#8731=DIRECTION('',(1.,0.,0.));
#8732=DIRECTION('',(0.,-1.,2.22044604925031E-16));
#8733=DIRECTION('',(1.,0.,0.));
#8734=DIRECTION('',(0.,0.,1.));
#8735=DIRECTION('',(1.,0.,0.));
#8736=DIRECTION('',(0.,-1.,2.22044604925031E-16));
#8737=DIRECTION('',(1.,0.,0.));
#8738=DIRECTION('',(0.,0.,1.));
#8739=DIRECTION('',(1.,0.,0.));
#8740=DIRECTION('',(0.,0.,1.));
#8741=DIRECTION('',(1.,0.,0.));
#8742=DIRECTION('',(0.,-1.,2.22044604925031E-16));
#8743=DIRECTION('',(1.,0.,0.));
#8744=DIRECTION('',(0.,0.,1.));
#8745=DIRECTION('',(1.,0.,0.));
#8746=DIRECTION('',(0.,-1.,2.22044604925031E-16));
#8747=DIRECTION('',(1.,0.,0.));
#8748=DIRECTION('',(0.,0.,1.));
#8749=DIRECTION('',(1.,0.,0.));
#8750=DIRECTION('',(0.,0.,1.));
#8751=DIRECTION('',(1.,0.,0.));
#8752=DIRECTION('',(0.,-1.,2.22044604925031E-16));
#8753=DIRECTION('',(1.,0.,0.));
#8754=DIRECTION('',(0.,0.,1.));
#8755=DIRECTION('',(1.,0.,0.));
#8756=DIRECTION('',(0.,-1.,2.22044604925031E-16));
#8757=DIRECTION('',(1.,0.,0.));
#8758=DIRECTION('',(0.,-1.,2.22044604925031E-16));
#8759=DIRECTION('',(1.,0.,0.));
#8760=DIRECTION('',(0.,-1.,2.22044604925031E-16));
#8761=DIRECTION('',(1.,0.,0.));
#8762=DIRECTION('',(0.,0.,1.));
#8763=DIRECTION('',(1.,0.,0.));
#8764=DIRECTION('',(0.,0.,1.));
#8765=DIRECTION('',(1.,0.,0.));
#8766=DIRECTION('',(0.,0.,1.));
#8767=DIRECTION('',(1.,0.,0.));
#8768=DIRECTION('',(0.,0.,1.));
#8769=DIRECTION('',(1.,0.,0.));
#8770=DIRECTION('',(0.,0.,1.));
#8771=DIRECTION('',(1.,0.,0.));
#8772=DIRECTION('',(0.,0.,1.));
#8773=DIRECTION('',(1.,0.,0.));
#8774=DIRECTION('',(0.,0.,1.));
#8775=DIRECTION('',(1.,0.,0.));
#8776=DIRECTION('',(0.,0.,1.));
#8777=DIRECTION('',(1.,0.,0.));
#8778=DIRECTION('',(0.,0.,1.));
#8779=DIRECTION('',(1.,0.,0.));
#8780=DIRECTION('',(0.,0.,1.));
#8781=DIRECTION('',(1.,0.,0.));
#8782=DIRECTION('',(0.,0.,1.));
#8783=DIRECTION('',(1.,0.,0.));
#8784=DIRECTION('',(0.,0.,1.));
#8785=DIRECTION('',(1.,0.,0.));
#8786=DIRECTION('',(0.,0.,1.));
#8787=DIRECTION('',(1.,0.,0.));
#8788=DIRECTION('',(0.,0.,1.));
#8789=DIRECTION('',(1.,0.,0.));
#8790=DIRECTION('',(0.,0.,1.));
#8791=DIRECTION('',(1.,0.,0.));
#8792=DIRECTION('',(0.,0.,1.));
#8793=DIRECTION('',(1.,0.,0.));
#8794=DIRECTION('',(0.,0.,1.));
#8795=DIRECTION('',(1.,0.,0.));
#8796=DIRECTION('',(0.,-1.,2.22044604925031E-16));
#8797=DIRECTION('',(1.,0.,0.));
#8798=DIRECTION('',(0.,-1.,2.22044604925031E-16));
#8799=DIRECTION('',(1.,0.,0.));
#8800=DIRECTION('',(0.,0.,1.));
#8801=DIRECTION('',(1.,0.,0.));
#8802=DIRECTION('',(0.,0.,1.));
#8803=DIRECTION('',(1.,0.,0.));
#8804=DIRECTION('',(0.,0.,1.));
#8805=DIRECTION('',(1.,0.,0.));
#8806=DIRECTION('',(0.,0.,1.));
#8807=DIRECTION('',(1.,0.,0.));
#8808=DIRECTION('',(0.,0.,1.));
#8809=DIRECTION('',(1.,0.,0.));
#8810=DIRECTION('',(0.,0.,1.));
#8811=DIRECTION('',(1.,0.,0.));
#8812=DIRECTION('',(0.,0.,1.));
#8813=DIRECTION('',(1.,0.,0.));
#8814=DIRECTION('',(0.,0.,1.));
#8815=DIRECTION('',(1.,0.,0.));
#8816=DIRECTION('',(0.,0.,1.));
#8817=DIRECTION('',(1.,0.,0.));
#8818=DIRECTION('',(0.,0.,1.));
#8819=DIRECTION('',(1.,0.,0.));
#8820=DIRECTION('',(0.,0.,1.));
#8821=DIRECTION('',(1.,0.,0.));
#8822=DIRECTION('',(0.,0.,1.));
#8823=DIRECTION('',(1.,0.,0.));
#8824=DIRECTION('',(0.,0.,1.));
#8825=DIRECTION('',(1.,0.,0.));
#8826=DIRECTION('',(0.,0.,1.));
#8827=DIRECTION('',(1.,0.,0.));
#8828=DIRECTION('',(0.,0.,1.));
#8829=DIRECTION('',(1.,0.,0.));
#8830=DIRECTION('',(0.,0.,1.));
#8831=DIRECTION('',(1.,0.,0.));
#8832=DIRECTION('',(0.,0.,1.));
#8833=DIRECTION('',(1.,0.,0.));
#8834=DIRECTION('axis',(0.,0.,1.));
#8835=DIRECTION('refdir',(1.,0.,0.));
#8836=DIRECTION('axis',(0.,0.,1.));
#8837=DIRECTION('refdir',(1.,0.,0.));
#8838=DIRECTION('center_axis',(-1.,0.,0.));
#8839=DIRECTION('ref_axis',(0.,0.,1.));
#8840=DIRECTION('',(0.,-1.,0.));
#8841=DIRECTION('',(0.,0.,1.));
#8842=DIRECTION('',(0.,1.,0.));
#8843=DIRECTION('',(0.,0.,-1.));
#8844=DIRECTION('center_axis',(0.,1.,0.));
#8845=DIRECTION('ref_axis',(1.,0.,0.));
#8846=DIRECTION('center_axis',(0.,-1.,0.));
#8847=DIRECTION('ref_axis',(1.,0.,0.));
#8848=DIRECTION('',(-1.,0.,0.));
#8849=DIRECTION('',(0.,0.,1.));
#8850=DIRECTION('center_axis',(1.,0.,0.));
#8851=DIRECTION('ref_axis',(0.,0.,-1.));
#8852=DIRECTION('',(0.,1.,0.));
#8853=DIRECTION('',(0.,1.,0.));
#8854=DIRECTION('',(0.,0.,-1.));
#8855=DIRECTION('center_axis',(0.,0.,1.));
#8856=DIRECTION('ref_axis',(1.,0.,0.));
#8857=DIRECTION('',(1.,0.,0.));
#8858=DIRECTION('center_axis',(0.,1.,0.));
#8859=DIRECTION('ref_axis',(0.,0.,1.));
#8860=DIRECTION('center_axis',(0.,1.,0.));
#8861=DIRECTION('ref_axis',(1.,0.,0.));
#8862=DIRECTION('center_axis',(0.,1.,0.));
#8863=DIRECTION('ref_axis',(1.,0.,0.));
#8864=DIRECTION('center_axis',(0.,1.,0.));
#8865=DIRECTION('ref_axis',(1.,0.,0.));
#8866=DIRECTION('center_axis',(0.,1.,0.));
#8867=DIRECTION('ref_axis',(1.,0.,0.));
#8868=DIRECTION('center_axis',(0.,1.,0.));
#8869=DIRECTION('ref_axis',(1.,0.,0.));
#8870=DIRECTION('center_axis',(0.,1.,0.));
#8871=DIRECTION('ref_axis',(1.,0.,0.));
#8872=DIRECTION('center_axis',(0.,-1.,0.));
#8873=DIRECTION('ref_axis',(1.,0.,0.));
#8874=DIRECTION('center_axis',(0.,1.,0.));
#8875=DIRECTION('ref_axis',(1.,0.,0.));
#8876=DIRECTION('',(0.,-1.,0.));
#8877=DIRECTION('center_axis',(0.,1.,0.));
#8878=DIRECTION('ref_axis',(1.,0.,0.));
#8879=DIRECTION('',(0.,-1.,0.));
#8880=DIRECTION('center_axis',(0.,1.,0.));
#8881=DIRECTION('ref_axis',(1.,0.,0.));
#8882=DIRECTION('center_axis',(0.,1.,0.));
#8883=DIRECTION('ref_axis',(1.,0.,0.));
#8884=DIRECTION('center_axis',(0.,1.,0.));
#8885=DIRECTION('ref_axis',(1.,0.,0.));
#8886=DIRECTION('',(0.,-1.,0.));
#8887=DIRECTION('center_axis',(0.,1.,0.));
#8888=DIRECTION('ref_axis',(1.,0.,0.));
#8889=DIRECTION('center_axis',(0.,1.,0.));
#8890=DIRECTION('ref_axis',(1.,0.,0.));
#8891=DIRECTION('axis',(0.,0.,1.));
#8892=DIRECTION('refdir',(1.,0.,0.));
#8893=DIRECTION('center_axis',(0.,1.,0.));
#8894=DIRECTION('ref_axis',(1.,0.,0.));
#8895=DIRECTION('center_axis',(0.,-1.,0.));
#8896=DIRECTION('ref_axis',(1.,0.,0.));
#8897=DIRECTION('',(0.,-1.,0.));
#8898=DIRECTION('center_axis',(0.,-1.,0.));
#8899=DIRECTION('ref_axis',(1.,0.,0.));
#8900=DIRECTION('center_axis',(0.,1.,0.));
#8901=DIRECTION('ref_axis',(1.,0.,0.));
#8902=DIRECTION('center_axis',(0.,1.,0.));
#8903=DIRECTION('ref_axis',(1.,0.,0.));
#8904=DIRECTION('',(0.,-1.,0.));
#8905=DIRECTION('center_axis',(0.,1.,0.));
#8906=DIRECTION('ref_axis',(1.,0.,0.));
#8907=DIRECTION('center_axis',(0.,1.,0.));
#8908=DIRECTION('ref_axis',(1.,0.,0.));
#8909=DIRECTION('center_axis',(0.,1.,0.));
#8910=DIRECTION('ref_axis',(1.,0.,0.));
#8911=DIRECTION('axis',(0.,0.,1.));
#8912=DIRECTION('refdir',(1.,0.,0.));
#8913=DIRECTION('center_axis',(0.,1.,0.));
#8914=DIRECTION('ref_axis',(1.,0.,0.));
#8915=DIRECTION('center_axis',(0.,-1.,0.));
#8916=DIRECTION('ref_axis',(1.,0.,0.));
#8917=DIRECTION('',(0.,-1.,0.));
#8918=DIRECTION('center_axis',(0.,-1.,0.));
#8919=DIRECTION('ref_axis',(1.,0.,0.));
#8920=DIRECTION('center_axis',(0.,1.,0.));
#8921=DIRECTION('ref_axis',(1.,0.,0.));
#8922=DIRECTION('center_axis',(0.,1.,0.));
#8923=DIRECTION('ref_axis',(1.,0.,0.));
#8924=DIRECTION('',(0.,-1.,0.));
#8925=DIRECTION('center_axis',(0.,1.,0.));
#8926=DIRECTION('ref_axis',(1.,0.,0.));
#8927=DIRECTION('center_axis',(0.,1.,0.));
#8928=DIRECTION('ref_axis',(1.,0.,0.));
#8929=DIRECTION('center_axis',(0.,1.,0.));
#8930=DIRECTION('ref_axis',(1.,0.,0.));
#8931=DIRECTION('axis',(0.,0.,1.));
#8932=DIRECTION('refdir',(1.,0.,0.));
#8933=DIRECTION('center_axis',(0.,1.,0.));
#8934=DIRECTION('ref_axis',(1.,0.,0.));
#8935=DIRECTION('center_axis',(0.,1.,0.));
#8936=DIRECTION('ref_axis',(1.,0.,0.));
#8937=DIRECTION('',(0.,1.,0.));
#8938=DIRECTION('center_axis',(0.,-1.,0.));
#8939=DIRECTION('ref_axis',(1.,0.,0.));
#8940=DIRECTION('center_axis',(0.866025403784439,0.,-0.5));
#8941=DIRECTION('ref_axis',(-0.5,0.,-0.866025403784439));
#8942=DIRECTION('',(0.5,0.,0.866025403784438));
#8943=DIRECTION('',(0.,1.,0.));
#8944=DIRECTION('',(-0.5,0.,-0.866025403784438));
#8945=DIRECTION('',(0.,1.,0.));
#8946=DIRECTION('center_axis',(0.866025403784439,0.,0.5));
#8947=DIRECTION('ref_axis',(0.5,0.,-0.866025403784439));
#8948=DIRECTION('',(-0.5,0.,0.866025403784438));
#8949=DIRECTION('',(0.5,0.,-0.866025403784438));
#8950=DIRECTION('',(0.,1.,0.));
#8951=DIRECTION('center_axis',(0.,0.,1.));
#8952=DIRECTION('ref_axis',(1.,0.,0.));
#8953=DIRECTION('',(-1.,0.,0.));
#8954=DIRECTION('',(1.,0.,0.));
#8955=DIRECTION('',(0.,1.,0.));
#8956=DIRECTION('center_axis',(-0.866025403784438,0.,0.5));
#8957=DIRECTION('ref_axis',(0.5,0.,0.866025403784438));
#8958=DIRECTION('',(-0.5,0.,-0.866025403784438));
#8959=DIRECTION('',(0.5,0.,0.866025403784438));
#8960=DIRECTION('',(0.,1.,0.));
#8961=DIRECTION('center_axis',(-0.866025403784439,0.,-0.5));
#8962=DIRECTION('ref_axis',(-0.5,0.,0.866025403784439));
#8963=DIRECTION('',(0.5,0.,-0.866025403784439));
#8964=DIRECTION('',(-0.5,0.,0.866025403784439));
#8965=DIRECTION('',(0.,1.,0.));
#8966=DIRECTION('center_axis',(0.,0.,-1.));
#8967=DIRECTION('ref_axis',(-1.,0.,0.));
#8968=DIRECTION('',(1.,0.,0.));
#8969=DIRECTION('',(-1.,0.,0.));
#8970=DIRECTION('center_axis',(0.,1.,0.));
#8971=DIRECTION('ref_axis',(0.,0.,1.));
#8972=DIRECTION('center_axis',(0.,1.,0.));
#8973=DIRECTION('ref_axis',(1.,0.,0.));
#8974=DIRECTION('axis',(0.,0.,1.));
#8975=DIRECTION('refdir',(1.,0.,0.));
#8976=DIRECTION('center_axis',(0.,1.,0.));
#8977=DIRECTION('ref_axis',(1.,0.,0.));
#8978=DIRECTION('center_axis',(0.,1.,0.));
#8979=DIRECTION('ref_axis',(1.,0.,0.));
#8980=DIRECTION('',(0.,1.,0.));
#8981=DIRECTION('center_axis',(0.,-1.,0.));
#8982=DIRECTION('ref_axis',(1.,0.,0.));
#8983=DIRECTION('center_axis',(0.866025403784439,0.,-0.5));
#8984=DIRECTION('ref_axis',(-0.5,0.,-0.866025403784439));
#8985=DIRECTION('',(0.5,0.,0.866025403784438));
#8986=DIRECTION('',(0.,1.,0.));
#8987=DIRECTION('',(-0.5,0.,-0.866025403784438));
#8988=DIRECTION('',(0.,1.,0.));
#8989=DIRECTION('center_axis',(0.866025403784439,0.,0.5));
#8990=DIRECTION('ref_axis',(0.5,0.,-0.866025403784439));
#8991=DIRECTION('',(-0.5,0.,0.866025403784438));
#8992=DIRECTION('',(0.5,0.,-0.866025403784438));
#8993=DIRECTION('',(0.,1.,0.));
#8994=DIRECTION('center_axis',(0.,0.,1.));
#8995=DIRECTION('ref_axis',(1.,0.,0.));
#8996=DIRECTION('',(-1.,0.,0.));
#8997=DIRECTION('',(1.,0.,0.));
#8998=DIRECTION('',(0.,1.,0.));
#8999=DIRECTION('center_axis',(-0.866025403784438,0.,0.5));
#9000=DIRECTION('ref_axis',(0.5,0.,0.866025403784438));
#9001=DIRECTION('',(-0.5,0.,-0.866025403784438));
#9002=DIRECTION('',(0.5,0.,0.866025403784438));
#9003=DIRECTION('',(0.,1.,0.));
#9004=DIRECTION('center_axis',(-0.866025403784439,0.,-0.5));
#9005=DIRECTION('ref_axis',(-0.5,0.,0.866025403784439));
#9006=DIRECTION('',(0.5,0.,-0.866025403784439));
#9007=DIRECTION('',(-0.5,0.,0.866025403784439));
#9008=DIRECTION('',(0.,1.,0.));
#9009=DIRECTION('center_axis',(0.,0.,-1.));
#9010=DIRECTION('ref_axis',(-1.,0.,0.));
#9011=DIRECTION('',(1.,0.,0.));
#9012=DIRECTION('',(-1.,0.,0.));
#9013=DIRECTION('center_axis',(0.,1.,0.));
#9014=DIRECTION('ref_axis',(0.,0.,1.));
#9015=DIRECTION('center_axis',(0.,1.,0.));
#9016=DIRECTION('ref_axis',(1.,0.,0.));
#9017=DIRECTION('axis',(0.,0.,1.));
#9018=DIRECTION('refdir',(1.,0.,0.));
#9019=DIRECTION('center_axis',(0.,0.,1.));
#9020=DIRECTION('ref_axis',(1.,0.,0.));
#9021=DIRECTION('',(0.,1.,0.));
#9022=DIRECTION('center_axis',(0.,0.,1.));
#9023=DIRECTION('ref_axis',(1.,0.,0.));
#9024=DIRECTION('center_axis',(0.,0.,1.));
#9025=DIRECTION('ref_axis',(1.,0.,0.));
#9026=DIRECTION('center_axis',(0.,0.,1.));
#9027=DIRECTION('ref_axis',(1.,0.,0.));
#9028=DIRECTION('',(0.,0.,1.));
#9029=DIRECTION('center_axis',(0.,0.,1.));
#9030=DIRECTION('ref_axis',(1.,0.,0.));
#9031=DIRECTION('center_axis',(0.,0.,1.));
#9032=DIRECTION('ref_axis',(1.,0.,0.));
#9033=DIRECTION('',(0.,-1.,0.));
#9034=DIRECTION('center_axis',(-1.,0.,0.));
#9035=DIRECTION('ref_axis',(0.,0.,1.));
#9036=DIRECTION('',(0.,0.,1.));
#9037=DIRECTION('',(0.,1.,0.));
#9038=DIRECTION('',(0.,0.,-1.));
#9039=DIRECTION('',(0.,1.,0.));
#9040=DIRECTION('center_axis',(0.,0.,-1.));
#9041=DIRECTION('ref_axis',(-1.,0.,0.));
#9042=DIRECTION('',(-1.,0.,0.));
#9043=DIRECTION('',(0.,1.,0.));
#9044=DIRECTION('',(1.,0.,0.));
#9045=DIRECTION('center_axis',(1.,0.,0.));
#9046=DIRECTION('ref_axis',(0.,0.,-1.));
#9047=DIRECTION('',(0.,0.,-1.));
#9048=DIRECTION('',(0.,-1.,0.));
#9049=DIRECTION('',(0.,0.,1.));
#9050=DIRECTION('center_axis',(0.,1.,0.));
#9051=DIRECTION('ref_axis',(1.,0.,0.));
#9052=DIRECTION('center_axis',(0.,1.,0.));
#9053=DIRECTION('ref_axis',(1.,0.,0.));
#9054=DIRECTION('center_axis',(0.,-1.,0.));
#9055=DIRECTION('ref_axis',(1.,0.,0.));
#9056=DIRECTION('center_axis',(0.,1.,0.));
#9057=DIRECTION('ref_axis',(-1.83697019872103E-16,0.,1.));
#9058=DIRECTION('center_axis',(0.,-1.,0.));
#9059=DIRECTION('ref_axis',(1.,0.,0.));
#9060=DIRECTION('center_axis',(0.,1.,0.));
#9061=DIRECTION('ref_axis',(1.,0.,0.));
#9062=DIRECTION('center_axis',(0.,1.,0.));
#9063=DIRECTION('ref_axis',(1.,0.,0.));
#9064=DIRECTION('',(0.,1.,0.));
#9065=DIRECTION('center_axis',(0.,-1.,0.));
#9066=DIRECTION('ref_axis',(1.,0.,0.));
#9067=DIRECTION('center_axis',(0.,1.,0.));
#9068=DIRECTION('ref_axis',(1.,0.,0.));
#9069=DIRECTION('center_axis',(0.,1.,0.));
#9070=DIRECTION('ref_axis',(1.,0.,0.));
#9071=DIRECTION('',(0.,1.,0.));
#9072=DIRECTION('center_axis',(0.,-1.,0.));
#9073=DIRECTION('ref_axis',(1.,0.,0.));
#9074=DIRECTION('center_axis',(0.,1.,0.));
#9075=DIRECTION('ref_axis',(1.,0.,0.));
#9076=DIRECTION('center_axis',(0.,1.,0.));
#9077=DIRECTION('ref_axis',(1.,0.,0.));
#9078=DIRECTION('',(0.,1.,0.));
#9079=DIRECTION('center_axis',(0.,-1.,0.));
#9080=DIRECTION('ref_axis',(1.,0.,0.));
#9081=DIRECTION('center_axis',(0.,1.,0.));
#9082=DIRECTION('ref_axis',(1.,0.,0.));
#9083=DIRECTION('center_axis',(0.,1.,0.));
#9084=DIRECTION('ref_axis',(1.,0.,0.));
#9085=DIRECTION('',(0.,1.,0.));
#9086=DIRECTION('center_axis',(0.,-1.,0.));
#9087=DIRECTION('ref_axis',(1.,0.,0.));
#9088=DIRECTION('center_axis',(0.,1.,0.));
#9089=DIRECTION('ref_axis',(1.,0.,0.));
#9090=DIRECTION('center_axis',(0.,1.,0.));
#9091=DIRECTION('ref_axis',(1.,0.,0.));
#9092=DIRECTION('center_axis',(0.,1.,0.));
#9093=DIRECTION('ref_axis',(1.,0.,0.));
#9094=DIRECTION('center_axis',(0.,1.,0.));
#9095=DIRECTION('ref_axis',(1.,0.,0.));
#9096=DIRECTION('center_axis',(0.,1.,0.));
#9097=DIRECTION('ref_axis',(1.,0.,0.));
#9098=DIRECTION('center_axis',(0.,-1.,0.));
#9099=DIRECTION('ref_axis',(1.,0.,0.));
#9100=DIRECTION('center_axis',(0.,1.,0.));
#9101=DIRECTION('ref_axis',(1.,0.,0.));
#9102=DIRECTION('',(0.,-1.,0.));
#9103=DIRECTION('center_axis',(0.,1.,0.));
#9104=DIRECTION('ref_axis',(1.,0.,0.));
#9105=DIRECTION('',(0.,-1.,0.));
#9106=DIRECTION('center_axis',(0.,1.,0.));
#9107=DIRECTION('ref_axis',(1.,0.,0.));
#9108=DIRECTION('center_axis',(0.,1.,0.));
#9109=DIRECTION('ref_axis',(1.,0.,0.));
#9110=DIRECTION('',(0.,-1.,0.));
#9111=DIRECTION('center_axis',(0.,1.,0.));
#9112=DIRECTION('ref_axis',(1.,0.,0.));
#9113=DIRECTION('axis',(0.,0.,1.));
#9114=DIRECTION('refdir',(1.,0.,0.));
#9115=DIRECTION('center_axis',(1.,0.,0.));
#9116=DIRECTION('ref_axis',(0.,0.,-1.));
#9117=DIRECTION('',(0.,0.707106781186547,-0.707106781186548));
#9118=DIRECTION('',(0.,1.,0.));
#9119=DIRECTION('',(0.,0.707106781186547,0.707106781186548));
#9120=DIRECTION('',(0.,0.,1.));
#9121=DIRECTION('',(0.,-0.707106781186548,0.707106781186548));
#9122=DIRECTION('',(0.,-1.,0.));
#9123=DIRECTION('',(0.,-0.707106781186548,-0.707106781186548));
#9124=DIRECTION('',(0.,0.,-1.));
#9125=DIRECTION('center_axis',(0.,-0.707106781186548,-0.707106781186548));
#9126=DIRECTION('ref_axis',(-1.,0.,0.));
#9127=DIRECTION('',(-1.,0.,0.));
#9128=DIRECTION('',(0.,0.707106781186548,-0.707106781186548));
#9129=DIRECTION('',(1.,0.,0.));
#9130=DIRECTION('center_axis',(0.,-1.,0.));
#9131=DIRECTION('ref_axis',(1.,0.,0.));
#9132=DIRECTION('',(1.,0.,0.));
#9133=DIRECTION('',(0.,0.,-1.));
#9134=DIRECTION('center_axis',(0.,-0.707106781186548,0.707106781186547));
#9135=DIRECTION('ref_axis',(1.,0.,0.));
#9136=DIRECTION('',(-1.,0.,0.));
#9137=DIRECTION('',(0.,-0.707106781186547,-0.707106781186548));
#9138=DIRECTION('center_axis',(0.,0.,1.));
#9139=DIRECTION('ref_axis',(1.,0.,0.));
#9140=DIRECTION('',(1.,0.,0.));
#9141=DIRECTION('',(0.,-1.,0.));
#9142=DIRECTION('center_axis',(1.,0.,0.));
#9143=DIRECTION('ref_axis',(0.,0.,-1.));
#9144=DIRECTION('',(0.,-0.707106781186547,0.707106781186548));
#9145=DIRECTION('',(0.,0.,1.));
#9146=DIRECTION('',(0.,0.707106781186548,0.707106781186548));
#9147=DIRECTION('',(0.,1.,0.));
#9148=DIRECTION('center_axis',(0.,0.707106781186548,0.707106781186547));
#9149=DIRECTION('ref_axis',(1.,0.,0.));
#9150=DIRECTION('',(-1.,0.,0.));
#9151=DIRECTION('center_axis',(0.,1.,0.));
#9152=DIRECTION('ref_axis',(-1.,0.,0.));
#9153=DIRECTION('',(1.,0.,0.));
#9154=DIRECTION('center_axis',(0.,0.707106781186548,-0.707106781186548));
#9155=DIRECTION('ref_axis',(-1.,0.,0.));
#9156=DIRECTION('',(-1.,0.,0.));
#9157=DIRECTION('center_axis',(0.,0.,1.));
#9158=DIRECTION('ref_axis',(1.,0.,0.));
#9159=DIRECTION('axis',(0.,0.,1.));
#9160=DIRECTION('refdir',(1.,0.,0.));
#9161=DIRECTION('center_axis',(0.866025403784439,0.,-0.5));
#9162=DIRECTION('ref_axis',(0.5,0.,0.866025403784439));
#9163=DIRECTION('',(0.5,0.,0.866025403784439));
#9164=DIRECTION('',(0.,-1.,0.));
#9165=DIRECTION('',(0.5,0.,0.866025403784439));
#9166=DIRECTION('',(0.,-1.,0.));
#9167=DIRECTION('center_axis',(1.92296268638356E-16,0.,-1.));
#9168=DIRECTION('ref_axis',(1.,0.,1.92296268638356E-16));
#9169=DIRECTION('',(1.,0.,1.92296268638356E-16));
#9170=DIRECTION('',(0.,-1.,0.));
#9171=DIRECTION('',(1.,0.,1.92296268638356E-16));
#9172=DIRECTION('center_axis',(-0.866025403784439,0.,-0.5));
#9173=DIRECTION('ref_axis',(0.5,0.,-0.866025403784439));
#9174=DIRECTION('',(0.5,0.,-0.866025403784439));
#9175=DIRECTION('',(0.,-1.,0.));
#9176=DIRECTION('',(0.5,0.,-0.866025403784438));
#9177=DIRECTION('center_axis',(-0.866025403784439,0.,0.5));
#9178=DIRECTION('ref_axis',(-0.5,0.,-0.866025403784439));
#9179=DIRECTION('',(-0.5,0.,-0.866025403784439));
#9180=DIRECTION('',(0.,-1.,0.));
#9181=DIRECTION('',(-0.5,0.,-0.866025403784439));
#9182=DIRECTION('center_axis',(-1.92296268638356E-16,0.,1.));
#9183=DIRECTION('ref_axis',(-1.,0.,-1.92296268638356E-16));
#9184=DIRECTION('',(-1.,0.,-1.92296268638356E-16));
#9185=DIRECTION('',(0.,-1.,0.));
#9186=DIRECTION('',(-1.,0.,-1.92296268638356E-16));
#9187=DIRECTION('center_axis',(0.866025403784439,0.,0.5));
#9188=DIRECTION('ref_axis',(-0.5,0.,0.866025403784439));
#9189=DIRECTION('',(-0.5,0.,0.866025403784439));
#9190=DIRECTION('',(-0.5,0.,0.866025403784439));
#9191=DIRECTION('center_axis',(0.,-1.,0.));
#9192=DIRECTION('ref_axis',(0.,0.,-1.));
#9193=DIRECTION('center_axis',(0.,1.,0.));
#9194=DIRECTION('ref_axis',(0.,0.,1.));
#9195=DIRECTION('center_axis',(0.,-1.,0.));
#9196=DIRECTION('ref_axis',(1.,0.,0.));
#9197=DIRECTION('center_axis',(0.,-1.,0.));
#9198=DIRECTION('ref_axis',(1.,0.,0.));
#9199=DIRECTION('center_axis',(0.,-1.,0.));
#9200=DIRECTION('ref_axis',(1.,0.,0.));
#9201=DIRECTION('',(0.707106781186547,0.707106781186548,8.65956056235493E-17));
#9202=DIRECTION('center_axis',(0.,-1.,0.));
#9203=DIRECTION('ref_axis',(1.,0.,0.));
#9204=DIRECTION('center_axis',(0.,1.,0.));
#9205=DIRECTION('ref_axis',(1.,0.,0.));
#9206=DIRECTION('',(0.,1.,0.));
#9207=DIRECTION('center_axis',(0.,1.,0.));
#9208=DIRECTION('ref_axis',(1.,0.,0.));
#9209=DIRECTION('center_axis',(0.,-1.,0.));
#9210=DIRECTION('ref_axis',(1.,0.,0.));
#9211=DIRECTION('',(-0.707106781186547,0.707106781186548,-8.65956056235493E-17));
#9212=DIRECTION('center_axis',(0.,-1.,0.));
#9213=DIRECTION('ref_axis',(0.,0.,-1.));
#9214=DIRECTION('',(0.,0.,1.));
#9215=DIRECTION('',(1.,0.,0.));
#9216=DIRECTION('',(0.,0.,1.));
#9217=DIRECTION('',(1.,0.,0.));
#9218=DIRECTION('',(0.,0.,1.));
#9219=DIRECTION('',(1.,0.,0.));
#9220=DIRECTION('',(0.,0.,1.));
#9221=DIRECTION('',(1.,0.,0.));
#9222=DIRECTION('',(0.,0.,1.));
#9223=DIRECTION('',(1.,0.,0.));
#9224=DIRECTION('',(0.,0.,1.));
#9225=DIRECTION('',(1.,0.,0.));
#9226=DIRECTION('',(8.65956056235493E-17,-8.65956056235493E-17,-1.));
#9227=DIRECTION('',(2.22044604925031E-16,1.,-8.65956056235494E-17));
#9228=DIRECTION('',(0.,-1.,2.22044604925031E-16));
#9229=DIRECTION('',(1.,0.,0.));
#9230=DIRECTION('',(0.,0.,1.));
#9231=DIRECTION('',(1.,0.,0.));
#9232=DIRECTION('',(0.,0.,1.));
#9233=DIRECTION('',(1.,0.,0.));
#9234=CARTESIAN_POINT('',(0.,0.,0.));
#9235=CARTESIAN_POINT('',(0.,0.,0.));
#9236=CARTESIAN_POINT('',(0.,0.,0.));
#9237=CARTESIAN_POINT('Origin',(-5.,15.5,1.9));
#9238=CARTESIAN_POINT('',(-5.25,15.5,2.));
#9239=CARTESIAN_POINT('Origin',(-5.,15.5,2.));
#9240=CARTESIAN_POINT('',(-5.25,15.5,3.2));
#9241=CARTESIAN_POINT('',(-5.25,15.5,1.9));
#9242=CARTESIAN_POINT('Origin',(-5.,15.5,3.2));
#9243=CARTESIAN_POINT('Origin',(5.,15.5,1.9));
#9244=CARTESIAN_POINT('',(4.75,15.5,2.));
#9245=CARTESIAN_POINT('Origin',(5.,15.5,2.));
#9246=CARTESIAN_POINT('',(4.75,15.5,3.2));
#9247=CARTESIAN_POINT('',(4.75,15.5,1.9));
#9248=CARTESIAN_POINT('Origin',(5.,15.5,3.2));
#9249=CARTESIAN_POINT('Origin',(-5.,-2.5,1.9));
#9250=CARTESIAN_POINT('',(-5.25,-2.5,2.));
#9251=CARTESIAN_POINT('Origin',(-5.,-2.5,2.));
#9252=CARTESIAN_POINT('',(-5.25,-2.5,3.2));
#9253=CARTESIAN_POINT('',(-5.25,-2.5,1.9));
#9254=CARTESIAN_POINT('Origin',(-5.,-2.5,3.2));
#9255=CARTESIAN_POINT('Origin',(5.,-2.5,1.9));
#9256=CARTESIAN_POINT('',(4.75,-2.5,2.));
#9257=CARTESIAN_POINT('Origin',(5.,-2.5,2.));
#9258=CARTESIAN_POINT('',(4.75,-2.5,3.2));
#9259=CARTESIAN_POINT('',(4.75,-2.5,1.9));
#9260=CARTESIAN_POINT('Origin',(5.,-2.5,3.2));
#9261=CARTESIAN_POINT('Origin',(7.,13.,1.9));
#9262=CARTESIAN_POINT('',(6.725,13.,2.));
#9263=CARTESIAN_POINT('Origin',(7.,13.,2.));
#9264=CARTESIAN_POINT('',(6.725,13.,3.2));
#9265=CARTESIAN_POINT('',(6.725,13.,1.9));
#9266=CARTESIAN_POINT('Origin',(7.,13.,3.2));
#9267=CARTESIAN_POINT('Origin',(7.,-3.,1.9));
#9268=CARTESIAN_POINT('',(6.725,-3.,2.));
#9269=CARTESIAN_POINT('Origin',(7.,-3.,2.));
#9270=CARTESIAN_POINT('',(6.725,-3.,3.2));
#9271=CARTESIAN_POINT('',(6.725,-3.,1.9));
#9272=CARTESIAN_POINT('Origin',(7.,-3.,3.2));
#9273=CARTESIAN_POINT('Origin',(-7.,21.,1.9));
#9274=CARTESIAN_POINT('',(-7.275,21.,2.));
#9275=CARTESIAN_POINT('Origin',(-7.,21.,2.));
#9276=CARTESIAN_POINT('',(-7.275,21.,3.2));
#9277=CARTESIAN_POINT('',(-7.275,21.,1.9));
#9278=CARTESIAN_POINT('Origin',(-7.,21.,3.2));
#9279=CARTESIAN_POINT('Origin',(-7.,5.,1.9));
#9280=CARTESIAN_POINT('',(-7.275,5.,2.));
#9281=CARTESIAN_POINT('Origin',(-7.,5.,2.));
#9282=CARTESIAN_POINT('',(-7.275,5.,3.2));
#9283=CARTESIAN_POINT('',(-7.275,5.,1.9));
#9284=CARTESIAN_POINT('Origin',(-7.,5.,3.2));
#9285=CARTESIAN_POINT('Origin',(-7.,13.,1.9));
#9286=CARTESIAN_POINT('',(-7.275,13.,2.));
#9287=CARTESIAN_POINT('Origin',(-7.,13.,2.));
#9288=CARTESIAN_POINT('',(-7.275,13.,3.2));
#9289=CARTESIAN_POINT('',(-7.275,13.,1.9));
#9290=CARTESIAN_POINT('Origin',(-7.,13.,3.2));
#9291=CARTESIAN_POINT('Origin',(-7.,-3.,1.9));
#9292=CARTESIAN_POINT('',(-7.275,-3.,2.));
#9293=CARTESIAN_POINT('Origin',(-7.,-3.,2.));
#9294=CARTESIAN_POINT('',(-7.275,-3.,3.2));
#9295=CARTESIAN_POINT('',(-7.275,-3.,1.9));
#9296=CARTESIAN_POINT('Origin',(-7.,-3.,3.2));
#9297=CARTESIAN_POINT('Origin',(7.,5.,1.9));
#9298=CARTESIAN_POINT('',(6.725,5.,2.));
#9299=CARTESIAN_POINT('Origin',(7.,5.,2.));
#9300=CARTESIAN_POINT('',(6.725,5.,3.2));
#9301=CARTESIAN_POINT('',(6.725,5.,1.9));
#9302=CARTESIAN_POINT('Origin',(7.,5.,3.2));
#9303=CARTESIAN_POINT('Origin',(7.,21.,1.9));
#9304=CARTESIAN_POINT('',(6.725,21.,2.));
#9305=CARTESIAN_POINT('Origin',(7.,21.,2.));
#9306=CARTESIAN_POINT('',(6.725,21.,3.2));
#9307=CARTESIAN_POINT('',(6.725,21.,1.9));
#9308=CARTESIAN_POINT('Origin',(7.,21.,3.2));
#9309=CARTESIAN_POINT('Origin',(10.,23.,2.));
#9310=CARTESIAN_POINT('',(10.,23.,2.));
#9311=CARTESIAN_POINT('',(-10.,23.,2.));
#9312=CARTESIAN_POINT('',(10.,23.,2.));
#9313=CARTESIAN_POINT('',(-10.,23.,3.2));
#9314=CARTESIAN_POINT('',(-10.,23.,2.));
#9315=CARTESIAN_POINT('',(10.,23.,3.2));
#9316=CARTESIAN_POINT('',(10.,23.,3.2));
#9317=CARTESIAN_POINT('',(10.,23.,2.));
#9318=CARTESIAN_POINT('Origin',(10.,-5.,2.));
#9319=CARTESIAN_POINT('',(10.,-5.,2.));
#9320=CARTESIAN_POINT('',(10.,-5.,2.));
#9321=CARTESIAN_POINT('',(10.,-5.,3.2));
#9322=CARTESIAN_POINT('',(10.,-5.,3.2));
#9323=CARTESIAN_POINT('',(10.,-5.,2.));
#9324=CARTESIAN_POINT('Origin',(-10.,-5.,2.));
#9325=CARTESIAN_POINT('',(-10.,-5.,2.));
#9326=CARTESIAN_POINT('',(-10.,-5.,2.));
#9327=CARTESIAN_POINT('',(-10.,-5.,3.2));
#9328=CARTESIAN_POINT('',(-10.,-5.,3.2));
#9329=CARTESIAN_POINT('',(-10.,-5.,2.));
#9330=CARTESIAN_POINT('Origin',(-10.,23.,2.));
#9331=CARTESIAN_POINT('',(-10.,23.,2.));
#9332=CARTESIAN_POINT('',(-10.,23.,3.2));
#9333=CARTESIAN_POINT('Origin',(0.,9.,3.2));
#9334=CARTESIAN_POINT('Origin',(0.,9.,2.));
#9335=CARTESIAN_POINT('',(0.,0.,0.));
#9336=CARTESIAN_POINT('Origin',(10.,-2.,-0.4));
#9337=CARTESIAN_POINT('',(10.,-2.,-0.4));
#9338=CARTESIAN_POINT('',(-10.,-2.,-0.4));
#9339=CARTESIAN_POINT('',(10.,-2.,-0.4));
#9340=CARTESIAN_POINT('',(-10.,-2.,0.));
#9341=CARTESIAN_POINT('',(-10.,-2.,-0.4));
#9342=CARTESIAN_POINT('',(10.,-2.,0.));
#9343=CARTESIAN_POINT('',(10.,-2.,0.));
#9344=CARTESIAN_POINT('',(10.,-2.,-0.4));
#9345=CARTESIAN_POINT('Origin',(10.,-4.,-0.4));
#9346=CARTESIAN_POINT('',(10.,-4.,-0.4));
#9347=CARTESIAN_POINT('',(10.,-4.,-0.4));
#9348=CARTESIAN_POINT('',(10.,-4.,0.));
#9349=CARTESIAN_POINT('',(10.,-4.,0.));
#9350=CARTESIAN_POINT('',(10.,-4.,-0.4));
#9351=CARTESIAN_POINT('Origin',(-10.,-4.,-0.4));
#9352=CARTESIAN_POINT('',(-10.,-4.,-0.4));
#9353=CARTESIAN_POINT('',(-10.,-4.,-0.4));
#9354=CARTESIAN_POINT('',(-10.,-4.,0.));
#9355=CARTESIAN_POINT('',(-10.,-4.,0.));
#9356=CARTESIAN_POINT('',(-10.,-4.,-0.4));
#9357=CARTESIAN_POINT('Origin',(-10.,-2.,-0.4));
#9358=CARTESIAN_POINT('',(-10.,-2.,-0.4));
#9359=CARTESIAN_POINT('',(-10.,-2.,0.));
#9360=CARTESIAN_POINT('Origin',(0.,-3.,0.));
#9361=CARTESIAN_POINT('Origin',(0.,-3.,-0.4));
#9362=CARTESIAN_POINT('',(0.,0.,0.));
#9363=CARTESIAN_POINT('Origin',(10.,6.,-0.4));
#9364=CARTESIAN_POINT('',(10.,6.,-0.4));
#9365=CARTESIAN_POINT('',(-10.,6.,-0.4));
#9366=CARTESIAN_POINT('',(10.,6.,-0.4));
#9367=CARTESIAN_POINT('',(-10.,6.,0.));
#9368=CARTESIAN_POINT('',(-10.,6.,-0.4));
#9369=CARTESIAN_POINT('',(10.,6.,0.));
#9370=CARTESIAN_POINT('',(10.,6.,0.));
#9371=CARTESIAN_POINT('',(10.,6.,-0.4));
#9372=CARTESIAN_POINT('Origin',(10.,4.,-0.4));
#9373=CARTESIAN_POINT('',(10.,4.,-0.4));
#9374=CARTESIAN_POINT('',(10.,4.,-0.4));
#9375=CARTESIAN_POINT('',(10.,4.,0.));
#9376=CARTESIAN_POINT('',(10.,4.,0.));
#9377=CARTESIAN_POINT('',(10.,4.,-0.4));
#9378=CARTESIAN_POINT('Origin',(-10.,4.,-0.4));
#9379=CARTESIAN_POINT('',(-10.,4.,-0.4));
#9380=CARTESIAN_POINT('',(-10.,4.,-0.4));
#9381=CARTESIAN_POINT('',(-10.,4.,0.));
#9382=CARTESIAN_POINT('',(-10.,4.,0.));
#9383=CARTESIAN_POINT('',(-10.,4.,-0.4));
#9384=CARTESIAN_POINT('Origin',(-10.,6.,-0.4));
#9385=CARTESIAN_POINT('',(-10.,6.,-0.4));
#9386=CARTESIAN_POINT('',(-10.,6.,0.));
#9387=CARTESIAN_POINT('Origin',(0.,5.,0.));
#9388=CARTESIAN_POINT('Origin',(0.,5.,-0.4));
#9389=CARTESIAN_POINT('',(0.,0.,0.));
#9390=CARTESIAN_POINT('Origin',(10.,14.,-0.4));
#9391=CARTESIAN_POINT('',(10.,14.,-0.4));
#9392=CARTESIAN_POINT('',(-10.,14.,-0.4));
#9393=CARTESIAN_POINT('',(10.,14.,-0.4));
#9394=CARTESIAN_POINT('',(-10.,14.,0.));
#9395=CARTESIAN_POINT('',(-10.,14.,-0.4));
#9396=CARTESIAN_POINT('',(10.,14.,0.));
#9397=CARTESIAN_POINT('',(10.,14.,0.));
#9398=CARTESIAN_POINT('',(10.,14.,-0.4));
#9399=CARTESIAN_POINT('Origin',(10.,12.,-0.4));
#9400=CARTESIAN_POINT('',(10.,12.,-0.4));
#9401=CARTESIAN_POINT('',(10.,12.,-0.4));
#9402=CARTESIAN_POINT('',(10.,12.,0.));
#9403=CARTESIAN_POINT('',(10.,12.,0.));
#9404=CARTESIAN_POINT('',(10.,12.,-0.4));
#9405=CARTESIAN_POINT('Origin',(-10.,12.,-0.4));
#9406=CARTESIAN_POINT('',(-10.,12.,-0.4));
#9407=CARTESIAN_POINT('',(-10.,12.,-0.4));
#9408=CARTESIAN_POINT('',(-10.,12.,0.));
#9409=CARTESIAN_POINT('',(-10.,12.,0.));
#9410=CARTESIAN_POINT('',(-10.,12.,-0.4));
#9411=CARTESIAN_POINT('Origin',(-10.,14.,-0.4));
#9412=CARTESIAN_POINT('',(-10.,14.,-0.4));
#9413=CARTESIAN_POINT('',(-10.,14.,0.));
#9414=CARTESIAN_POINT('Origin',(0.,13.,0.));
#9415=CARTESIAN_POINT('Origin',(0.,13.,-0.4));
#9416=CARTESIAN_POINT('',(0.,0.,0.));
#9417=CARTESIAN_POINT('Origin',(10.,22.,-0.4));
#9418=CARTESIAN_POINT('',(10.,22.,-0.4));
#9419=CARTESIAN_POINT('',(-10.,22.,-0.4));
#9420=CARTESIAN_POINT('',(10.,22.,-0.4));
#9421=CARTESIAN_POINT('',(-10.,22.,0.));
#9422=CARTESIAN_POINT('',(-10.,22.,-0.4));
#9423=CARTESIAN_POINT('',(10.,22.,0.));
#9424=CARTESIAN_POINT('',(10.,22.,0.));
#9425=CARTESIAN_POINT('',(10.,22.,-0.4));
#9426=CARTESIAN_POINT('Origin',(10.,20.,-0.4));
#9427=CARTESIAN_POINT('',(10.,20.,-0.4));
#9428=CARTESIAN_POINT('',(10.,20.,-0.4));
#9429=CARTESIAN_POINT('',(10.,20.,0.));
#9430=CARTESIAN_POINT('',(10.,20.,0.));
#9431=CARTESIAN_POINT('',(10.,20.,-0.4));
#9432=CARTESIAN_POINT('Origin',(-10.,20.,-0.4));
#9433=CARTESIAN_POINT('',(-10.,20.,-0.4));
#9434=CARTESIAN_POINT('',(-10.,20.,-0.4));
#9435=CARTESIAN_POINT('',(-10.,20.,0.));
#9436=CARTESIAN_POINT('',(-10.,20.,0.));
#9437=CARTESIAN_POINT('',(-10.,20.,-0.4));
#9438=CARTESIAN_POINT('Origin',(-10.,22.,-0.4));
#9439=CARTESIAN_POINT('',(-10.,22.,-0.4));
#9440=CARTESIAN_POINT('',(-10.,22.,0.));
#9441=CARTESIAN_POINT('Origin',(0.,21.,0.));
#9442=CARTESIAN_POINT('Origin',(0.,21.,-0.4));
#9443=CARTESIAN_POINT('',(0.,0.,0.));
#9444=CARTESIAN_POINT('Origin',(-5.,-2.5,3.1));
#9445=CARTESIAN_POINT('',(-5.33,-2.5,3.2));
#9446=CARTESIAN_POINT('Origin',(-5.,-2.5,3.2));
#9447=CARTESIAN_POINT('',(-5.33,-2.5,4.2));
#9448=CARTESIAN_POINT('',(-5.33,-2.5,3.1));
#9449=CARTESIAN_POINT('Origin',(-5.,-2.5,4.2));
#9450=CARTESIAN_POINT('Origin',(5.,-2.5,3.1));
#9451=CARTESIAN_POINT('',(4.67,-2.5,3.2));
#9452=CARTESIAN_POINT('Origin',(5.,-2.5,3.2));
#9453=CARTESIAN_POINT('',(4.67,-2.5,4.2));
#9454=CARTESIAN_POINT('',(4.67,-2.5,3.1));
#9455=CARTESIAN_POINT('Origin',(5.,-2.5,4.2));
#9456=CARTESIAN_POINT('Origin',(3.2,-1.4,6.8));
#9457=CARTESIAN_POINT('',(2.76,-1.3,6.8));
#9458=CARTESIAN_POINT('Origin',(3.2,-1.3,6.8));
#9459=CARTESIAN_POINT('',(2.76,-0.5,6.8));
#9460=CARTESIAN_POINT('',(2.76,-1.4,6.8));
#9461=CARTESIAN_POINT('Origin',(3.2,-0.5,6.8));
#9462=CARTESIAN_POINT('Origin',(-3.2,-1.4,13.2));
#9463=CARTESIAN_POINT('',(-3.64,-1.3,13.2));
#9464=CARTESIAN_POINT('Origin',(-3.2,-1.3,13.2));
#9465=CARTESIAN_POINT('',(-3.64,-0.5,13.2));
#9466=CARTESIAN_POINT('',(-3.64,-1.4,13.2));
#9467=CARTESIAN_POINT('Origin',(-3.2,-0.5,13.2));
#9468=CARTESIAN_POINT('Origin',(-3.2,-1.4,6.8));
#9469=CARTESIAN_POINT('',(-3.64,-1.3,6.8));
#9470=CARTESIAN_POINT('Origin',(-3.2,-1.3,6.8));
#9471=CARTESIAN_POINT('',(-3.64,-0.5,6.8));
#9472=CARTESIAN_POINT('',(-3.64,-1.4,6.8));
#9473=CARTESIAN_POINT('Origin',(-3.2,-0.5,6.8));
#9474=CARTESIAN_POINT('Origin',(3.2,-1.4,13.2));
#9475=CARTESIAN_POINT('',(2.76,-1.3,13.2));
#9476=CARTESIAN_POINT('Origin',(3.2,-1.3,13.2));
#9477=CARTESIAN_POINT('',(2.76,-0.5,13.2));
#9478=CARTESIAN_POINT('',(2.76,-1.4,13.2));
#9479=CARTESIAN_POINT('Origin',(3.2,-0.5,13.2));
#9480=CARTESIAN_POINT('Origin',(0.,-1.4,10.));
#9481=CARTESIAN_POINT('',(-3.1,-1.3,10.));
#9482=CARTESIAN_POINT('Origin',(0.,-1.3,10.));
#9483=CARTESIAN_POINT('',(-3.1,-0.5,10.));
#9484=CARTESIAN_POINT('',(-3.1,-1.4,10.));
#9485=CARTESIAN_POINT('Origin',(0.,-0.5,10.));
#9486=CARTESIAN_POINT('Origin',(-6.5,-3.5,4.2));
#9487=CARTESIAN_POINT('',(-6.5,-1.3,4.2));
#9488=CARTESIAN_POINT('',(6.5,-1.3,4.2));
#9489=CARTESIAN_POINT('',(-6.5,-1.3,4.2));
#9490=CARTESIAN_POINT('',(-6.5,-3.5,4.2));
#9491=CARTESIAN_POINT('',(-6.5,-3.5,4.2));
#9492=CARTESIAN_POINT('',(6.5,-3.5,4.2));
#9493=CARTESIAN_POINT('',(6.5,-3.5,4.2));
#9494=CARTESIAN_POINT('',(6.5,-3.5,4.2));
#9495=CARTESIAN_POINT('Origin',(0.,-3.5,3.7));
#9496=CARTESIAN_POINT('',(-6.5,-3.5,3.2));
#9497=CARTESIAN_POINT('',(-6.5,-3.5,4.2));
#9498=CARTESIAN_POINT('',(6.5,-3.5,3.2));
#9499=CARTESIAN_POINT('',(-6.5,-3.5,3.2));
#9500=CARTESIAN_POINT('',(6.5,-3.5,3.2));
#9501=CARTESIAN_POINT('Origin',(6.5,-0.5,3.2));
#9502=CARTESIAN_POINT('',(-6.5,-0.5,3.2));
#9503=CARTESIAN_POINT('',(-6.5,-0.5,16.5));
#9504=CARTESIAN_POINT('',(-6.5,-0.5,3.2));
#9505=CARTESIAN_POINT('',(6.5,-0.5,16.5));
#9506=CARTESIAN_POINT('',(6.5,-0.5,16.5));
#9507=CARTESIAN_POINT('',(6.5,-0.5,3.2));
#9508=CARTESIAN_POINT('',(6.5,-0.5,3.2));
#9509=CARTESIAN_POINT('',(6.5,-0.5,3.2));
#9510=CARTESIAN_POINT('Origin',(-6.5,-0.5,3.2));
#9511=CARTESIAN_POINT('',(-6.5,-1.3,16.5));
#9512=CARTESIAN_POINT('',(-6.5,-1.3,3.2));
#9513=CARTESIAN_POINT('',(-6.5,-0.5,16.5));
#9514=CARTESIAN_POINT('',(-6.5,-0.5,3.2));
#9515=CARTESIAN_POINT('Origin',(6.5,-1.3,3.2));
#9516=CARTESIAN_POINT('',(6.5,-1.3,16.5));
#9517=CARTESIAN_POINT('',(6.5,-1.3,16.5));
#9518=CARTESIAN_POINT('',(6.5,-1.3,3.2));
#9519=CARTESIAN_POINT('',(6.5,-3.5,3.2));
#9520=CARTESIAN_POINT('Origin',(-6.5,-1.3,3.2));
#9521=CARTESIAN_POINT('',(-6.5,-1.3,16.5));
#9522=CARTESIAN_POINT('Origin',(0.,-0.9,16.5));
#9523=CARTESIAN_POINT('Origin',(0.,-0.9,3.2));
#9524=CARTESIAN_POINT('',(0.,0.,0.));
#9525=CARTESIAN_POINT('Origin',(-3.2,-0.5,6.8));
#9526=CARTESIAN_POINT('',(-3.625,0.5,6.8));
#9527=CARTESIAN_POINT('Origin',(-3.2,0.5,6.8));
#9528=CARTESIAN_POINT('',(-3.625,-0.5,6.8));
#9529=CARTESIAN_POINT('',(-3.625,-0.5,6.8));
#9530=CARTESIAN_POINT('Origin',(-3.2,-0.5,6.8));
#9531=CARTESIAN_POINT('Origin',(-3.2,-0.5,6.8));
#9532=CARTESIAN_POINT('',(-3.795,0.5,6.8));
#9533=CARTESIAN_POINT('Origin',(-3.2,0.5,6.8));
#9534=CARTESIAN_POINT('',(-3.795,-0.5,6.8));
#9535=CARTESIAN_POINT('',(-3.795,-0.5,6.8));
#9536=CARTESIAN_POINT('Origin',(-3.2,-0.5,6.8));
#9537=CARTESIAN_POINT('Origin',(-3.2,0.5,6.8));
#9538=CARTESIAN_POINT('Origin',(-3.2,-0.5,6.8));
#9539=CARTESIAN_POINT('',(0.,0.,0.));
#9540=CARTESIAN_POINT('Origin',(-3.2,-0.5,13.2));
#9541=CARTESIAN_POINT('',(-3.625,0.5,13.2));
#9542=CARTESIAN_POINT('Origin',(-3.2,0.5,13.2));
#9543=CARTESIAN_POINT('',(-3.625,-0.5,13.2));
#9544=CARTESIAN_POINT('',(-3.625,-0.5,13.2));
#9545=CARTESIAN_POINT('Origin',(-3.2,-0.5,13.2));
#9546=CARTESIAN_POINT('Origin',(-3.2,-0.5,13.2));
#9547=CARTESIAN_POINT('',(-3.795,0.5,13.2));
#9548=CARTESIAN_POINT('Origin',(-3.2,0.5,13.2));
#9549=CARTESIAN_POINT('',(-3.795,-0.5,13.2));
#9550=CARTESIAN_POINT('',(-3.795,-0.5,13.2));
#9551=CARTESIAN_POINT('Origin',(-3.2,-0.5,13.2));
#9552=CARTESIAN_POINT('Origin',(-3.2,0.5,13.2));
#9553=CARTESIAN_POINT('Origin',(-3.2,-0.5,13.2));
#9554=CARTESIAN_POINT('',(0.,0.,0.));
#9555=CARTESIAN_POINT('Origin',(3.2,-0.5,6.8));
#9556=CARTESIAN_POINT('',(2.775,0.5,6.8));
#9557=CARTESIAN_POINT('Origin',(3.2,0.5,6.8));
#9558=CARTESIAN_POINT('',(2.775,-0.5,6.8));
#9559=CARTESIAN_POINT('',(2.775,-0.5,6.8));
#9560=CARTESIAN_POINT('Origin',(3.2,-0.5,6.8));
#9561=CARTESIAN_POINT('Origin',(3.2,-0.5,6.8));
#9562=CARTESIAN_POINT('',(2.605,0.5,6.8));
#9563=CARTESIAN_POINT('Origin',(3.2,0.5,6.8));
#9564=CARTESIAN_POINT('',(2.605,-0.5,6.8));
#9565=CARTESIAN_POINT('',(2.605,-0.5,6.8));
#9566=CARTESIAN_POINT('Origin',(3.2,-0.5,6.8));
#9567=CARTESIAN_POINT('Origin',(3.2,0.5,6.8));
#9568=CARTESIAN_POINT('Origin',(3.2,-0.5,6.8));
#9569=CARTESIAN_POINT('',(0.,0.,0.));
#9570=CARTESIAN_POINT('Origin',(3.2,-0.5,13.2));
#9571=CARTESIAN_POINT('',(2.775,0.5,13.2));
#9572=CARTESIAN_POINT('Origin',(3.2,0.5,13.2));
#9573=CARTESIAN_POINT('',(2.775,-0.5,13.2));
#9574=CARTESIAN_POINT('',(2.775,-0.5,13.2));
#9575=CARTESIAN_POINT('Origin',(3.2,-0.5,13.2));
#9576=CARTESIAN_POINT('Origin',(3.2,-0.5,13.2));
#9577=CARTESIAN_POINT('',(2.605,0.5,13.2));
#9578=CARTESIAN_POINT('Origin',(3.2,0.5,13.2));
#9579=CARTESIAN_POINT('',(2.605,-0.5,13.2));
#9580=CARTESIAN_POINT('',(2.605,-0.5,13.2));
#9581=CARTESIAN_POINT('Origin',(3.2,-0.5,13.2));
#9582=CARTESIAN_POINT('Origin',(3.2,0.5,13.2));
#9583=CARTESIAN_POINT('Origin',(3.2,-0.5,13.2));
#9584=CARTESIAN_POINT('',(0.,0.,0.));
#9585=CARTESIAN_POINT('Origin',(-5.,15.5,3.1));
#9586=CARTESIAN_POINT('',(-5.33,15.5,3.2));
#9587=CARTESIAN_POINT('Origin',(-5.,15.5,3.2));
#9588=CARTESIAN_POINT('',(-5.33,15.5,4.2));
#9589=CARTESIAN_POINT('',(-5.33,15.5,3.1));
#9590=CARTESIAN_POINT('Origin',(-5.,15.5,4.2));
#9591=CARTESIAN_POINT('Origin',(5.,15.5,3.1));
#9592=CARTESIAN_POINT('',(4.67,15.5,3.2));
#9593=CARTESIAN_POINT('Origin',(5.,15.5,3.2));
#9594=CARTESIAN_POINT('',(4.67,15.5,4.2));
#9595=CARTESIAN_POINT('',(4.67,15.5,3.1));
#9596=CARTESIAN_POINT('Origin',(5.,15.5,4.2));
#9597=CARTESIAN_POINT('Origin',(3.2,16.6,6.8));
#9598=CARTESIAN_POINT('',(2.76,16.7,6.8));
#9599=CARTESIAN_POINT('Origin',(3.2,16.7,6.8));
#9600=CARTESIAN_POINT('',(2.76,17.5,6.8));
#9601=CARTESIAN_POINT('',(2.76,16.6,6.8));
#9602=CARTESIAN_POINT('Origin',(3.2,17.5,6.8));
#9603=CARTESIAN_POINT('Origin',(-3.2,16.6,13.2));
#9604=CARTESIAN_POINT('',(-3.64,16.7,13.2));
#9605=CARTESIAN_POINT('Origin',(-3.2,16.7,13.2));
#9606=CARTESIAN_POINT('',(-3.64,17.5,13.2));
#9607=CARTESIAN_POINT('',(-3.64,16.6,13.2));
#9608=CARTESIAN_POINT('Origin',(-3.2,17.5,13.2));
#9609=CARTESIAN_POINT('Origin',(-3.2,16.6,6.8));
#9610=CARTESIAN_POINT('',(-3.64,16.7,6.8));
#9611=CARTESIAN_POINT('Origin',(-3.2,16.7,6.8));
#9612=CARTESIAN_POINT('',(-3.64,17.5,6.8));
#9613=CARTESIAN_POINT('',(-3.64,16.6,6.8));
#9614=CARTESIAN_POINT('Origin',(-3.2,17.5,6.8));
#9615=CARTESIAN_POINT('Origin',(3.2,16.6,13.2));
#9616=CARTESIAN_POINT('',(2.76,16.7,13.2));
#9617=CARTESIAN_POINT('Origin',(3.2,16.7,13.2));
#9618=CARTESIAN_POINT('',(2.76,17.5,13.2));
#9619=CARTESIAN_POINT('',(2.76,16.6,13.2));
#9620=CARTESIAN_POINT('Origin',(3.2,17.5,13.2));
#9621=CARTESIAN_POINT('Origin',(0.,16.6,10.));
#9622=CARTESIAN_POINT('',(-3.1,16.7,10.));
#9623=CARTESIAN_POINT('Origin',(0.,16.7,10.));
#9624=CARTESIAN_POINT('',(-3.1,17.5,10.));
#9625=CARTESIAN_POINT('',(-3.1,16.6,10.));
#9626=CARTESIAN_POINT('Origin',(0.,17.5,10.));
#9627=CARTESIAN_POINT('Origin',(-6.5,14.5,4.2));
#9628=CARTESIAN_POINT('',(-6.5,16.7,4.2));
#9629=CARTESIAN_POINT('',(6.5,16.7,4.2));
#9630=CARTESIAN_POINT('',(-6.5,16.7,4.2));
#9631=CARTESIAN_POINT('',(-6.5,14.5,4.2));
#9632=CARTESIAN_POINT('',(-6.5,14.5,4.2));
#9633=CARTESIAN_POINT('',(6.5,14.5,4.2));
#9634=CARTESIAN_POINT('',(6.5,14.5,4.2));
#9635=CARTESIAN_POINT('',(6.5,14.5,4.2));
#9636=CARTESIAN_POINT('Origin',(0.,14.5,3.7));
#9637=CARTESIAN_POINT('',(-6.5,14.5,3.2));
#9638=CARTESIAN_POINT('',(-6.5,14.5,4.2));
#9639=CARTESIAN_POINT('',(6.5,14.5,3.2));
#9640=CARTESIAN_POINT('',(-6.5,14.5,3.2));
#9641=CARTESIAN_POINT('',(6.5,14.5,3.2));
#9642=CARTESIAN_POINT('Origin',(6.5,17.5,3.2));
#9643=CARTESIAN_POINT('',(-6.5,17.5,3.2));
#9644=CARTESIAN_POINT('',(-6.5,17.5,16.5));
#9645=CARTESIAN_POINT('',(-6.5,17.5,3.2));
#9646=CARTESIAN_POINT('',(6.5,17.5,16.5));
#9647=CARTESIAN_POINT('',(6.5,17.5,16.5));
#9648=CARTESIAN_POINT('',(6.5,17.5,3.2));
#9649=CARTESIAN_POINT('',(6.5,17.5,3.2));
#9650=CARTESIAN_POINT('',(6.5,17.5,3.2));
#9651=CARTESIAN_POINT('Origin',(-6.5,17.5,3.2));
#9652=CARTESIAN_POINT('',(-6.5,16.7,16.5));
#9653=CARTESIAN_POINT('',(-6.5,16.7,3.2));
#9654=CARTESIAN_POINT('',(-6.5,17.5,16.5));
#9655=CARTESIAN_POINT('',(-6.5,17.5,3.2));
#9656=CARTESIAN_POINT('Origin',(6.5,16.7,3.2));
#9657=CARTESIAN_POINT('',(6.5,16.7,16.5));
#9658=CARTESIAN_POINT('',(6.5,16.7,16.5));
#9659=CARTESIAN_POINT('',(6.5,16.7,3.2));
#9660=CARTESIAN_POINT('',(6.5,14.5,3.2));
#9661=CARTESIAN_POINT('Origin',(-6.5,16.7,3.2));
#9662=CARTESIAN_POINT('',(-6.5,16.7,16.5));
#9663=CARTESIAN_POINT('Origin',(0.,17.1,16.5));
#9664=CARTESIAN_POINT('Origin',(0.,17.1,3.2));
#9665=CARTESIAN_POINT('',(0.,0.,0.));
#9666=CARTESIAN_POINT('Origin',(-3.2,17.5,6.8));
#9667=CARTESIAN_POINT('',(-3.625,18.5,6.8));
#9668=CARTESIAN_POINT('Origin',(-3.2,18.5,6.8));
#9669=CARTESIAN_POINT('',(-3.625,17.5,6.8));
#9670=CARTESIAN_POINT('',(-3.625,17.5,6.8));
#9671=CARTESIAN_POINT('Origin',(-3.2,17.5,6.8));
#9672=CARTESIAN_POINT('Origin',(-3.2,17.5,6.8));
#9673=CARTESIAN_POINT('',(-3.795,18.5,6.8));
#9674=CARTESIAN_POINT('Origin',(-3.2,18.5,6.8));
#9675=CARTESIAN_POINT('',(-3.795,17.5,6.8));
#9676=CARTESIAN_POINT('',(-3.795,17.5,6.8));
#9677=CARTESIAN_POINT('Origin',(-3.2,17.5,6.8));
#9678=CARTESIAN_POINT('Origin',(-3.2,18.5,6.8));
#9679=CARTESIAN_POINT('Origin',(-3.2,17.5,6.8));
#9680=CARTESIAN_POINT('',(0.,0.,0.));
#9681=CARTESIAN_POINT('Origin',(-3.2,17.5,13.2));
#9682=CARTESIAN_POINT('',(-3.625,18.5,13.2));
#9683=CARTESIAN_POINT('Origin',(-3.2,18.5,13.2));
#9684=CARTESIAN_POINT('',(-3.625,17.5,13.2));
#9685=CARTESIAN_POINT('',(-3.625,17.5,13.2));
#9686=CARTESIAN_POINT('Origin',(-3.2,17.5,13.2));
#9687=CARTESIAN_POINT('Origin',(-3.2,17.5,13.2));
#9688=CARTESIAN_POINT('',(-3.795,18.5,13.2));
#9689=CARTESIAN_POINT('Origin',(-3.2,18.5,13.2));
#9690=CARTESIAN_POINT('',(-3.795,17.5,13.2));
#9691=CARTESIAN_POINT('',(-3.795,17.5,13.2));
#9692=CARTESIAN_POINT('Origin',(-3.2,17.5,13.2));
#9693=CARTESIAN_POINT('Origin',(-3.2,18.5,13.2));
#9694=CARTESIAN_POINT('Origin',(-3.2,17.5,13.2));
#9695=CARTESIAN_POINT('',(0.,0.,0.));
#9696=CARTESIAN_POINT('Origin',(3.2,17.5,6.8));
#9697=CARTESIAN_POINT('',(2.775,18.5,6.8));
#9698=CARTESIAN_POINT('Origin',(3.2,18.5,6.8));
#9699=CARTESIAN_POINT('',(2.775,17.5,6.8));
#9700=CARTESIAN_POINT('',(2.775,17.5,6.8));
#9701=CARTESIAN_POINT('Origin',(3.2,17.5,6.8));
#9702=CARTESIAN_POINT('Origin',(3.2,17.5,6.8));
#9703=CARTESIAN_POINT('',(2.605,18.5,6.8));
#9704=CARTESIAN_POINT('Origin',(3.2,18.5,6.8));
#9705=CARTESIAN_POINT('',(2.605,17.5,6.8));
#9706=CARTESIAN_POINT('',(2.605,17.5,6.8));
#9707=CARTESIAN_POINT('Origin',(3.2,17.5,6.8));
#9708=CARTESIAN_POINT('Origin',(3.2,18.5,6.8));
#9709=CARTESIAN_POINT('Origin',(3.2,17.5,6.8));
#9710=CARTESIAN_POINT('',(0.,0.,0.));
#9711=CARTESIAN_POINT('Origin',(3.2,17.5,13.2));
#9712=CARTESIAN_POINT('',(2.775,18.5,13.2));
#9713=CARTESIAN_POINT('Origin',(3.2,18.5,13.2));
#9714=CARTESIAN_POINT('',(2.775,17.5,13.2));
#9715=CARTESIAN_POINT('',(2.775,17.5,13.2));
#9716=CARTESIAN_POINT('Origin',(3.2,17.5,13.2));
#9717=CARTESIAN_POINT('Origin',(3.2,17.5,13.2));
#9718=CARTESIAN_POINT('',(2.605,18.5,13.2));
#9719=CARTESIAN_POINT('Origin',(3.2,18.5,13.2));
#9720=CARTESIAN_POINT('',(2.605,17.5,13.2));
#9721=CARTESIAN_POINT('',(2.605,17.5,13.2));
#9722=CARTESIAN_POINT('Origin',(3.2,17.5,13.2));
#9723=CARTESIAN_POINT('Origin',(3.2,18.5,13.2));
#9724=CARTESIAN_POINT('Origin',(3.2,17.5,13.2));
#9725=CARTESIAN_POINT('',(0.,0.,0.));
#9726=CARTESIAN_POINT('Origin',(-0.1,0.82,-0.3));
#9727=CARTESIAN_POINT('',(0.,0.82,-0.3));
#9728=CARTESIAN_POINT('',(0.,1.,-0.3));
#9729=CARTESIAN_POINT('',(0.,0.41,-0.3));
#9730=CARTESIAN_POINT('',(20.,0.82,-0.3));
#9731=CARTESIAN_POINT('',(-0.1,0.82,-0.3));
#9732=CARTESIAN_POINT('',(20.,1.,-0.3));
#9733=CARTESIAN_POINT('',(20.,0.41,-0.3));
#9734=CARTESIAN_POINT('',(-0.05,1.,-0.3));
#9735=CARTESIAN_POINT('Origin',(-0.1,0.82,-0.55));
#9736=CARTESIAN_POINT('',(0.,0.82,-0.55));
#9737=CARTESIAN_POINT('',(0.,0.82,-0.275));
#9738=CARTESIAN_POINT('',(20.,0.82,-0.55));
#9739=CARTESIAN_POINT('',(-0.1,0.82,-0.55));
#9740=CARTESIAN_POINT('',(20.,0.82,-0.275));
#9741=CARTESIAN_POINT('Origin',(-0.1,0.67,-0.55));
#9742=CARTESIAN_POINT('',(0.,0.67,-0.55));
#9743=CARTESIAN_POINT('',(0.,0.335,-0.55));
#9744=CARTESIAN_POINT('',(20.,0.67,-0.55));
#9745=CARTESIAN_POINT('',(-0.1,0.67,-0.55));
#9746=CARTESIAN_POINT('',(20.,0.335,-0.55));
#9747=CARTESIAN_POINT('Origin',(-0.1,0.42,-0.3));
#9748=CARTESIAN_POINT('',(0.,0.42,-0.3));
#9749=CARTESIAN_POINT('',(0.,0.24,-0.12));
#9750=CARTESIAN_POINT('',(20.,0.42,-0.3));
#9751=CARTESIAN_POINT('',(-0.1,0.42,-0.3));
#9752=CARTESIAN_POINT('',(20.,0.24,-0.12));
#9753=CARTESIAN_POINT('Origin',(-0.1,0.42,0.3));
#9754=CARTESIAN_POINT('',(0.,0.42,0.3));
#9755=CARTESIAN_POINT('',(0.,0.42,0.15));
#9756=CARTESIAN_POINT('',(20.,0.42,0.3));
#9757=CARTESIAN_POINT('',(-0.1,0.42,0.3));
#9758=CARTESIAN_POINT('',(20.,0.42,0.15));
#9759=CARTESIAN_POINT('Origin',(-0.1,0.67,0.55));
#9760=CARTESIAN_POINT('',(0.,0.67,0.55));
#9761=CARTESIAN_POINT('',(6.93889390390723E-18,0.365,0.245));
#9762=CARTESIAN_POINT('',(20.,0.67,0.55));
#9763=CARTESIAN_POINT('',(-0.1,0.67,0.55));
#9764=CARTESIAN_POINT('',(20.,0.365,0.245));
#9765=CARTESIAN_POINT('Origin',(-0.1,0.82,0.55));
#9766=CARTESIAN_POINT('',(0.,0.82,0.55));
#9767=CARTESIAN_POINT('',(0.,0.41,0.55));
#9768=CARTESIAN_POINT('',(20.,0.82,0.55));
#9769=CARTESIAN_POINT('',(-0.1,0.82,0.55));
#9770=CARTESIAN_POINT('',(20.,0.41,0.55));
#9771=CARTESIAN_POINT('Origin',(-0.1,0.82,0.3));
#9772=CARTESIAN_POINT('',(0.,0.82,0.3));
#9773=CARTESIAN_POINT('',(0.,0.82,0.15));
#9774=CARTESIAN_POINT('',(20.,0.82,0.3));
#9775=CARTESIAN_POINT('',(-0.1,0.82,0.3));
#9776=CARTESIAN_POINT('',(20.,0.82,0.15));
#9777=CARTESIAN_POINT('Origin',(-0.1,1.05,0.3));
#9778=CARTESIAN_POINT('',(0.,1.,0.3));
#9779=CARTESIAN_POINT('',(0.,0.525,0.3));
#9780=CARTESIAN_POINT('',(20.,1.,0.3));
#9781=CARTESIAN_POINT('',(-0.05,1.,0.3));
#9782=CARTESIAN_POINT('',(20.,0.525,0.3));
#9783=CARTESIAN_POINT('Origin',(-0.1,-0.3,-0.82));
#9784=CARTESIAN_POINT('',(0.,-0.3,-0.82));
#9785=CARTESIAN_POINT('',(0.,-0.3,-1.));
#9786=CARTESIAN_POINT('',(0.,-0.3,-0.41));
#9787=CARTESIAN_POINT('',(20.,-0.3,-0.82));
#9788=CARTESIAN_POINT('',(-0.1,-0.3,-0.82));
#9789=CARTESIAN_POINT('',(20.,-0.3,-1.));
#9790=CARTESIAN_POINT('',(20.,-0.3,-0.41));
#9791=CARTESIAN_POINT('',(-0.05,-0.3,-1.));
#9792=CARTESIAN_POINT('Origin',(-0.1,-0.55,-0.82));
#9793=CARTESIAN_POINT('',(0.,-0.55,-0.82));
#9794=CARTESIAN_POINT('',(0.,-0.275,-0.82));
#9795=CARTESIAN_POINT('',(20.,-0.55,-0.82));
#9796=CARTESIAN_POINT('',(-0.1,-0.55,-0.82));
#9797=CARTESIAN_POINT('',(20.,-0.275,-0.82));
#9798=CARTESIAN_POINT('Origin',(-0.1,-0.55,-0.67));
#9799=CARTESIAN_POINT('',(0.,-0.55,-0.67));
#9800=CARTESIAN_POINT('',(0.,-0.55,-0.335));
#9801=CARTESIAN_POINT('',(20.,-0.55,-0.67));
#9802=CARTESIAN_POINT('',(-0.1,-0.55,-0.67));
#9803=CARTESIAN_POINT('',(20.,-0.55,-0.335));
#9804=CARTESIAN_POINT('Origin',(-0.1,-0.3,-0.42));
#9805=CARTESIAN_POINT('',(0.,-0.3,-0.42));
#9806=CARTESIAN_POINT('',(0.,-0.12,-0.24));
#9807=CARTESIAN_POINT('',(20.,-0.3,-0.42));
#9808=CARTESIAN_POINT('',(-0.1,-0.3,-0.42));
#9809=CARTESIAN_POINT('',(20.,-0.12,-0.24));
#9810=CARTESIAN_POINT('Origin',(-0.1,0.3,-0.42));
#9811=CARTESIAN_POINT('',(0.,0.3,-0.42));
#9812=CARTESIAN_POINT('',(0.,0.15,-0.42));
#9813=CARTESIAN_POINT('',(20.,0.3,-0.42));
#9814=CARTESIAN_POINT('',(-0.1,0.3,-0.42));
#9815=CARTESIAN_POINT('',(20.,0.15,-0.42));
#9816=CARTESIAN_POINT('Origin',(-0.1,0.55,-0.67));
#9817=CARTESIAN_POINT('',(0.,0.55,-0.67));
#9818=CARTESIAN_POINT('',(0.,0.245,-0.365));
#9819=CARTESIAN_POINT('',(20.,0.55,-0.67));
#9820=CARTESIAN_POINT('',(-0.1,0.55,-0.67));
#9821=CARTESIAN_POINT('',(20.,0.245,-0.365));
#9822=CARTESIAN_POINT('Origin',(-0.1,0.55,-0.82));
#9823=CARTESIAN_POINT('',(0.,0.55,-0.82));
#9824=CARTESIAN_POINT('',(0.,0.55,-0.41));
#9825=CARTESIAN_POINT('',(20.,0.55,-0.82));
#9826=CARTESIAN_POINT('',(-0.1,0.55,-0.82));
#9827=CARTESIAN_POINT('',(20.,0.55,-0.41));
#9828=CARTESIAN_POINT('Origin',(-0.1,0.3,-0.82));
#9829=CARTESIAN_POINT('',(0.,0.3,-0.82));
#9830=CARTESIAN_POINT('',(0.,0.15,-0.82));
#9831=CARTESIAN_POINT('',(20.,0.3,-0.82));
#9832=CARTESIAN_POINT('',(-0.1,0.3,-0.82));
#9833=CARTESIAN_POINT('',(20.,0.15,-0.82));
#9834=CARTESIAN_POINT('Origin',(-0.1,0.3,-1.05));
#9835=CARTESIAN_POINT('',(0.,0.3,-1.));
#9836=CARTESIAN_POINT('',(0.,0.3,-0.525));
#9837=CARTESIAN_POINT('',(20.,0.3,-1.));
#9838=CARTESIAN_POINT('',(-0.05,0.3,-1.));
#9839=CARTESIAN_POINT('',(20.,0.3,-0.525));
#9840=CARTESIAN_POINT('Origin',(-0.1,-0.82,0.3));
#9841=CARTESIAN_POINT('',(0.,-0.82,0.3));
#9842=CARTESIAN_POINT('',(0.,-1.,0.3));
#9843=CARTESIAN_POINT('',(0.,-0.41,0.3));
#9844=CARTESIAN_POINT('',(20.,-0.82,0.3));
#9845=CARTESIAN_POINT('',(-0.1,-0.82,0.3));
#9846=CARTESIAN_POINT('',(20.,-1.,0.3));
#9847=CARTESIAN_POINT('',(20.,-0.41,0.3));
#9848=CARTESIAN_POINT('',(-0.05,-1.,0.3));
#9849=CARTESIAN_POINT('Origin',(-0.1,-0.82,0.55));
#9850=CARTESIAN_POINT('',(0.,-0.82,0.55));
#9851=CARTESIAN_POINT('',(0.,-0.82,0.275));
#9852=CARTESIAN_POINT('',(20.,-0.82,0.55));
#9853=CARTESIAN_POINT('',(-0.1,-0.82,0.55));
#9854=CARTESIAN_POINT('',(20.,-0.82,0.275));
#9855=CARTESIAN_POINT('Origin',(-0.1,-0.67,0.55));
#9856=CARTESIAN_POINT('',(0.,-0.67,0.55));
#9857=CARTESIAN_POINT('',(0.,-0.335,0.55));
#9858=CARTESIAN_POINT('',(20.,-0.67,0.55));
#9859=CARTESIAN_POINT('',(-0.1,-0.67,0.55));
#9860=CARTESIAN_POINT('',(20.,-0.335,0.55));
#9861=CARTESIAN_POINT('Origin',(-0.1,-0.42,0.3));
#9862=CARTESIAN_POINT('',(0.,-0.42,0.3));
#9863=CARTESIAN_POINT('',(-6.93889390390723E-18,-0.24,0.12));
#9864=CARTESIAN_POINT('',(20.,-0.42,0.3));
#9865=CARTESIAN_POINT('',(-0.1,-0.42,0.3));
#9866=CARTESIAN_POINT('',(20.,-0.24,0.12));
#9867=CARTESIAN_POINT('Origin',(-0.1,-0.42,-0.3));
#9868=CARTESIAN_POINT('',(0.,-0.42,-0.3));
#9869=CARTESIAN_POINT('',(0.,-0.42,-0.15));
#9870=CARTESIAN_POINT('',(20.,-0.42,-0.3));
#9871=CARTESIAN_POINT('',(-0.1,-0.42,-0.3));
#9872=CARTESIAN_POINT('',(20.,-0.42,-0.15));
#9873=CARTESIAN_POINT('Origin',(-0.1,-0.67,-0.55));
#9874=CARTESIAN_POINT('',(0.,-0.67,-0.55));
#9875=CARTESIAN_POINT('',(0.,-0.365,-0.245));
#9876=CARTESIAN_POINT('',(20.,-0.67,-0.55));
#9877=CARTESIAN_POINT('',(-0.1,-0.67,-0.55));
#9878=CARTESIAN_POINT('',(20.,-0.365,-0.245));
#9879=CARTESIAN_POINT('Origin',(-0.1,-0.82,-0.55));
#9880=CARTESIAN_POINT('',(0.,-0.82,-0.55));
#9881=CARTESIAN_POINT('',(0.,-0.41,-0.55));
#9882=CARTESIAN_POINT('',(20.,-0.82,-0.55));
#9883=CARTESIAN_POINT('',(-0.1,-0.82,-0.55));
#9884=CARTESIAN_POINT('',(20.,-0.41,-0.55));
#9885=CARTESIAN_POINT('Origin',(-0.1,-0.82,-0.3));
#9886=CARTESIAN_POINT('',(0.,-0.82,-0.3));
#9887=CARTESIAN_POINT('',(0.,-0.82,-0.15));
#9888=CARTESIAN_POINT('',(20.,-0.82,-0.3));
#9889=CARTESIAN_POINT('',(-0.1,-0.82,-0.3));
#9890=CARTESIAN_POINT('',(20.,-0.82,-0.15));
#9891=CARTESIAN_POINT('Origin',(-0.1,-1.05,-0.3));
#9892=CARTESIAN_POINT('',(0.,-1.,-0.3));
#9893=CARTESIAN_POINT('',(0.,-0.525,-0.3));
#9894=CARTESIAN_POINT('',(20.,-1.,-0.3));
#9895=CARTESIAN_POINT('',(-0.05,-1.,-0.3));
#9896=CARTESIAN_POINT('',(20.,-0.525,-0.3));
#9897=CARTESIAN_POINT('Origin',(-0.1,0.3,0.82));
#9898=CARTESIAN_POINT('',(0.,0.3,0.82));
#9899=CARTESIAN_POINT('',(0.,0.3,1.));
#9900=CARTESIAN_POINT('',(0.,0.3,0.41));
#9901=CARTESIAN_POINT('',(20.,0.3,0.82));
#9902=CARTESIAN_POINT('',(-0.1,0.3,0.82));
#9903=CARTESIAN_POINT('',(20.,0.3,1.));
#9904=CARTESIAN_POINT('',(20.,0.3,0.41));
#9905=CARTESIAN_POINT('',(-0.05,0.3,1.));
#9906=CARTESIAN_POINT('Origin',(-0.1,0.55,0.82));
#9907=CARTESIAN_POINT('',(0.,0.55,0.82));
#9908=CARTESIAN_POINT('',(0.,0.275,0.82));
#9909=CARTESIAN_POINT('',(20.,0.55,0.82));
#9910=CARTESIAN_POINT('',(-0.1,0.55,0.82));
#9911=CARTESIAN_POINT('',(20.,0.275,0.82));
#9912=CARTESIAN_POINT('Origin',(-0.1,0.55,0.67));
#9913=CARTESIAN_POINT('',(0.,0.55,0.67));
#9914=CARTESIAN_POINT('',(0.,0.55,0.335));
#9915=CARTESIAN_POINT('',(20.,0.55,0.67));
#9916=CARTESIAN_POINT('',(-0.1,0.55,0.67));
#9917=CARTESIAN_POINT('',(20.,0.55,0.335));
#9918=CARTESIAN_POINT('Origin',(-0.1,0.3,0.42));
#9919=CARTESIAN_POINT('',(0.,0.3,0.42));
#9920=CARTESIAN_POINT('',(6.93889390390723E-18,0.12,0.24));
#9921=CARTESIAN_POINT('',(20.,0.3,0.42));
#9922=CARTESIAN_POINT('',(-0.1,0.3,0.42));
#9923=CARTESIAN_POINT('',(20.,0.12,0.24));
#9924=CARTESIAN_POINT('Origin',(-0.1,-0.3,0.42));
#9925=CARTESIAN_POINT('',(0.,-0.3,0.42));
#9926=CARTESIAN_POINT('',(0.,-0.15,0.42));
#9927=CARTESIAN_POINT('',(20.,-0.3,0.42));
#9928=CARTESIAN_POINT('',(-0.1,-0.3,0.42));
#9929=CARTESIAN_POINT('',(20.,-0.15,0.42));
#9930=CARTESIAN_POINT('Origin',(-0.1,-0.55,0.67));
#9931=CARTESIAN_POINT('',(0.,-0.55,0.67));
#9932=CARTESIAN_POINT('',(6.93889390390723E-18,-0.245,0.365));
#9933=CARTESIAN_POINT('',(20.,-0.55,0.67));
#9934=CARTESIAN_POINT('',(-0.1,-0.55,0.67));
#9935=CARTESIAN_POINT('',(20.,-0.245,0.365));
#9936=CARTESIAN_POINT('Origin',(-0.1,-0.55,0.82));
#9937=CARTESIAN_POINT('',(0.,-0.55,0.82));
#9938=CARTESIAN_POINT('',(0.,-0.55,0.41));
#9939=CARTESIAN_POINT('',(20.,-0.55,0.82));
#9940=CARTESIAN_POINT('',(-0.1,-0.55,0.82));
#9941=CARTESIAN_POINT('',(20.,-0.55,0.41));
#9942=CARTESIAN_POINT('Origin',(-0.1,-0.3,0.82));
#9943=CARTESIAN_POINT('',(0.,-0.3,0.82));
#9944=CARTESIAN_POINT('',(0.,-0.15,0.82));
#9945=CARTESIAN_POINT('',(20.,-0.3,0.82));
#9946=CARTESIAN_POINT('',(-0.1,-0.3,0.82));
#9947=CARTESIAN_POINT('',(20.,-0.15,0.82));
#9948=CARTESIAN_POINT('Origin',(-0.1,-0.3,1.05));
#9949=CARTESIAN_POINT('',(0.,-0.3,1.));
#9950=CARTESIAN_POINT('',(0.,-0.3,0.525));
#9951=CARTESIAN_POINT('',(20.,-0.3,1.));
#9952=CARTESIAN_POINT('',(-0.05,-0.3,1.));
#9953=CARTESIAN_POINT('',(20.,-0.3,0.525));
#9954=CARTESIAN_POINT('Origin',(-0.1,0.,0.));
#9955=CARTESIAN_POINT('',(0.,-2.57175827820944E-17,0.21));
#9956=CARTESIAN_POINT('Origin',(0.,0.,0.));
#9957=CARTESIAN_POINT('',(20.,2.57175827820944E-17,0.21));
#9958=CARTESIAN_POINT('',(-0.1,-2.57175827820944E-17,0.21));
#9959=CARTESIAN_POINT('Origin',(20.,0.,0.));
#9960=CARTESIAN_POINT('Origin',(0.,1.,-1.));
#9961=CARTESIAN_POINT('',(0.,1.,1.));
#9962=CARTESIAN_POINT('',(0.,1.,-1.));
#9963=CARTESIAN_POINT('',(20.,1.,1.));
#9964=CARTESIAN_POINT('',(0.,1.,1.));
#9965=CARTESIAN_POINT('',(20.,1.,-1.));
#9966=CARTESIAN_POINT('Origin',(0.,1.,-1.));
#9967=CARTESIAN_POINT('',(20.,1.,-1.));
#9968=CARTESIAN_POINT('',(20.,1.,-1.));
#9969=CARTESIAN_POINT('',(0.,1.,-1.));
#9970=CARTESIAN_POINT('',(0.,1.,-1.));
#9971=CARTESIAN_POINT('',(0.,1.,-1.));
#9972=CARTESIAN_POINT('Origin',(0.,-1.,-1.));
#9973=CARTESIAN_POINT('',(0.,-1.,-1.));
#9974=CARTESIAN_POINT('',(20.,-1.,-1.));
#9975=CARTESIAN_POINT('Origin',(0.,-1.,-1.));
#9976=CARTESIAN_POINT('',(20.,-1.,-1.));
#9977=CARTESIAN_POINT('',(20.,-1.,-1.));
#9978=CARTESIAN_POINT('',(0.,-1.,-1.));
#9979=CARTESIAN_POINT('',(0.,-1.,-1.));
#9980=CARTESIAN_POINT('',(0.,-1.,-1.));
#9981=CARTESIAN_POINT('Origin',(0.,-1.,1.));
#9982=CARTESIAN_POINT('',(0.,-1.,1.));
#9983=CARTESIAN_POINT('',(20.,-1.,1.));
#9984=CARTESIAN_POINT('Origin',(0.,-1.,1.));
#9985=CARTESIAN_POINT('',(20.,-1.,1.));
#9986=CARTESIAN_POINT('',(20.,-1.,1.));
#9987=CARTESIAN_POINT('',(0.,-1.,1.));
#9988=CARTESIAN_POINT('',(0.,-1.,1.));
#9989=CARTESIAN_POINT('',(0.,-1.,1.));
#9990=CARTESIAN_POINT('Origin',(0.,1.,1.));
#9991=CARTESIAN_POINT('',(0.,1.,1.));
#9992=CARTESIAN_POINT('',(20.,1.,1.));
#9993=CARTESIAN_POINT('Origin',(0.,1.,1.));
#9994=CARTESIAN_POINT('',(20.,1.,1.));
#9995=CARTESIAN_POINT('',(0.,1.,1.));
#9996=CARTESIAN_POINT('Origin',(20.,0.,0.));
#9997=CARTESIAN_POINT('Origin',(0.,0.,0.));
#9998=CARTESIAN_POINT('',(0.,0.,0.));
#9999=CARTESIAN_POINT('Origin',(0.,0.395,0.25));
#10000=CARTESIAN_POINT('',(-0.5,0.3,0.25));
#10001=CARTESIAN_POINT('',(0.5,0.3,0.25));
#10002=CARTESIAN_POINT('',(0.25,0.3,0.25));
#10003=CARTESIAN_POINT('',(-0.5,0.5,0.25));
#10004=CARTESIAN_POINT('',(-0.5,0.5,0.25));
#10005=CARTESIAN_POINT('',(0.5,0.5,0.25));
#10006=CARTESIAN_POINT('',(0.5,0.5,0.25));
#10007=CARTESIAN_POINT('',(0.5,0.29,0.25));
#10008=CARTESIAN_POINT('Origin',(0.5,0.5,0.25));
#10009=CARTESIAN_POINT('',(-0.5,0.5,0.4));
#10010=CARTESIAN_POINT('',(-0.5,0.5,0.25));
#10011=CARTESIAN_POINT('',(0.5,0.5,0.4));
#10012=CARTESIAN_POINT('',(0.5,0.5,0.4));
#10013=CARTESIAN_POINT('',(0.5,0.5,0.25));
#10014=CARTESIAN_POINT('Origin',(0.,0.,0.4));
#10015=CARTESIAN_POINT('',(-0.5,-0.5,0.4));
#10016=CARTESIAN_POINT('',(-0.5,0.5,0.4));
#10017=CARTESIAN_POINT('',(0.5,-0.5,0.4));
#10018=CARTESIAN_POINT('',(-0.5,-0.5,0.4));
#10019=CARTESIAN_POINT('',(0.5,-0.3,0.4));
#10020=CARTESIAN_POINT('',(-0.2117,2.59257727379495E-17,0.4));
#10021=CARTESIAN_POINT('Origin',(0.,0.,0.4));
#10022=CARTESIAN_POINT('Origin',(-0.5,0.3,0.));
#10023=CARTESIAN_POINT('',(-0.5,0.3,0.15));
#10024=CARTESIAN_POINT('',(-0.5,0.3,0.));
#10025=CARTESIAN_POINT('',(-0.5,0.15,0.));
#10026=CARTESIAN_POINT('',(-0.5,0.225,0.075));
#10027=CARTESIAN_POINT('',(-0.5,-0.15,0.));
#10028=CARTESIAN_POINT('',(-0.5,0.3,0.));
#10029=CARTESIAN_POINT('',(-0.5,-0.3,0.15));
#10030=CARTESIAN_POINT('',(-0.5,-0.075,-0.075));
#10031=CARTESIAN_POINT('',(-0.5,-0.3,0.25));
#10032=CARTESIAN_POINT('',(-0.5,-0.3,0.));
#10033=CARTESIAN_POINT('',(-0.5,-0.5,0.25));
#10034=CARTESIAN_POINT('',(-0.5,-0.29,0.25));
#10035=CARTESIAN_POINT('',(-0.5,-0.5,0.25));
#10036=CARTESIAN_POINT('Origin',(-0.5,-0.5,0.25));
#10037=CARTESIAN_POINT('',(0.5,-0.5,0.25));
#10038=CARTESIAN_POINT('',(-0.5,-0.5,0.25));
#10039=CARTESIAN_POINT('',(0.5,-0.5,0.25));
#10040=CARTESIAN_POINT('Origin',(0.,-0.395,0.25));
#10041=CARTESIAN_POINT('',(0.5,-0.3,0.25));
#10042=CARTESIAN_POINT('',(-0.25,-0.3,0.25));
#10043=CARTESIAN_POINT('',(0.5,-0.5,0.25));
#10044=CARTESIAN_POINT('Origin',(0.5,-0.3,0.));
#10045=CARTESIAN_POINT('',(0.5,-0.3,0.15));
#10046=CARTESIAN_POINT('',(0.5,-0.3,0.));
#10047=CARTESIAN_POINT('',(0.5,-0.15,0.));
#10048=CARTESIAN_POINT('',(0.5,-0.225,0.075));
#10049=CARTESIAN_POINT('',(0.5,0.15,0.));
#10050=CARTESIAN_POINT('',(0.5,-0.3,0.));
#10051=CARTESIAN_POINT('',(0.5,0.3,0.15));
#10052=CARTESIAN_POINT('',(0.5,0.075,-0.075));
#10053=CARTESIAN_POINT('',(0.5,0.3,0.));
#10054=CARTESIAN_POINT('Origin',(-0.5,-0.3,0.));
#10055=CARTESIAN_POINT('',(-0.25,-0.3,0.15));
#10056=CARTESIAN_POINT('Origin',(-0.25,-0.225,0.075));
#10057=CARTESIAN_POINT('',(-0.149388386429468,-0.15,0.));
#10058=CARTESIAN_POINT('',(-0.25,-0.15,0.));
#10059=CARTESIAN_POINT('',(0.149388386429468,-0.15,0.));
#10060=CARTESIAN_POINT('Origin',(0.,0.,-0.15));
#10061=CARTESIAN_POINT('',(-0.25,-0.15,0.));
#10062=CARTESIAN_POINT('Origin',(0.,0.,-0.1));
#10063=CARTESIAN_POINT('',(-0.2117,-2.59257727379495E-17,0.));
#10064=CARTESIAN_POINT('Origin',(0.,0.,0.));
#10065=CARTESIAN_POINT('',(-0.2117,-2.59257727379495E-17,-0.1));
#10066=CARTESIAN_POINT('',(-0.149388386429468,0.15,0.));
#10067=CARTESIAN_POINT('Origin',(0.,0.,0.));
#10068=CARTESIAN_POINT('',(0.149388386429468,0.15,0.));
#10069=CARTESIAN_POINT('Origin',(0.,0.,-0.15));
#10070=CARTESIAN_POINT('Origin',(0.,0.,0.));
#10071=CARTESIAN_POINT('Origin',(0.,0.,0.));
#10072=CARTESIAN_POINT('',(0.25,0.15,0.));
#10073=CARTESIAN_POINT('Origin',(0.,0.,0.));
#10074=CARTESIAN_POINT('',(0.25,0.15,0.));
#10075=CARTESIAN_POINT('Origin',(0.25,0.225,0.075));
#10076=CARTESIAN_POINT('',(0.25,0.3,0.15));
#10077=CARTESIAN_POINT('Origin',(0.5,0.3,0.));
#10078=CARTESIAN_POINT('',(0.,0.,0.));
#10079=CARTESIAN_POINT('Origin',(0.115470053837925,-0.5,-0.2));
#10080=CARTESIAN_POINT('',(0.23094010767585,-0.5,0.));
#10081=CARTESIAN_POINT('',(0.115470053837925,-0.5,-0.2));
#10082=CARTESIAN_POINT('',(0.23094010767585,-0.5,0.));
#10083=CARTESIAN_POINT('',(0.115470053837925,-0.8,-0.2));
#10084=CARTESIAN_POINT('',(0.115470053837925,-0.5,-0.2));
#10085=CARTESIAN_POINT('',(0.23094010767585,-0.8,0.));
#10086=CARTESIAN_POINT('',(0.23094010767585,-0.8,0.));
#10087=CARTESIAN_POINT('',(0.23094010767585,-0.5,0.));
#10088=CARTESIAN_POINT('Origin',(-0.115470053837925,-0.5,-0.2));
#10089=CARTESIAN_POINT('',(-0.115470053837925,-0.5,-0.2));
#10090=CARTESIAN_POINT('',(0.115470053837925,-0.5,-0.2));
#10091=CARTESIAN_POINT('',(-0.115470053837925,-0.8,-0.2));
#10092=CARTESIAN_POINT('',(-0.115470053837925,-0.5,-0.2));
#10093=CARTESIAN_POINT('',(0.115470053837925,-0.8,-0.2));
#10094=CARTESIAN_POINT('Origin',(-0.23094010767585,-0.5,-2.77555756156289E-17));
#10095=CARTESIAN_POINT('',(-0.23094010767585,-0.5,-2.82820063659975E-17));
#10096=CARTESIAN_POINT('',(-0.115470053837925,-0.5,-0.2));
#10097=CARTESIAN_POINT('',(-0.23094010767585,-0.8,-2.77555756156289E-17));
#10098=CARTESIAN_POINT('',(-0.23094010767585,-0.5,-2.82820063659975E-17));
#10099=CARTESIAN_POINT('',(-0.115470053837925,-0.8,-0.2));
#10100=CARTESIAN_POINT('Origin',(-0.115470053837925,-0.5,0.2));
#10101=CARTESIAN_POINT('',(-0.115470053837925,-0.5,0.2));
#10102=CARTESIAN_POINT('',(-0.23094010767585,-0.5,-2.82820063659975E-17));
#10103=CARTESIAN_POINT('',(-0.115470053837925,-0.8,0.2));
#10104=CARTESIAN_POINT('',(-0.115470053837925,-0.5,0.2));
#10105=CARTESIAN_POINT('',(-0.23094010767585,-0.8,-2.82820063659975E-17));
#10106=CARTESIAN_POINT('Origin',(0.115470053837925,-0.5,0.2));
#10107=CARTESIAN_POINT('',(0.115470053837925,-0.5,0.2));
#10108=CARTESIAN_POINT('',(-0.115470053837925,-0.5,0.2));
#10109=CARTESIAN_POINT('',(0.115470053837925,-0.8,0.2));
#10110=CARTESIAN_POINT('',(0.115470053837925,-0.5,0.2));
#10111=CARTESIAN_POINT('',(-0.115470053837925,-0.8,0.2));
#10112=CARTESIAN_POINT('Origin',(0.23094010767585,-0.5,0.));
#10113=CARTESIAN_POINT('',(0.115470053837925,-0.5,0.2));
#10114=CARTESIAN_POINT('',(0.115470053837925,-0.8,0.2));
#10115=CARTESIAN_POINT('Origin',(0.,-0.5,0.));
#10116=CARTESIAN_POINT('Origin',(0.,-0.8,0.));
#10117=CARTESIAN_POINT('Origin',(0.,-1.7,0.));
#10118=CARTESIAN_POINT('',(-0.24505,-1.7,3.00099698131059E-17));
#10119=CARTESIAN_POINT('Origin',(0.,-1.7,0.));
#10120=CARTESIAN_POINT('Origin',(0.375,0.5,0.));
#10121=CARTESIAN_POINT('',(-0.375,0.5,-4.59242549680257E-17));
#10122=CARTESIAN_POINT('Origin',(0.,0.5,0.));
#10123=CARTESIAN_POINT('Origin',(0.,0.475,0.));
#10124=CARTESIAN_POINT('',(-0.425,0.45,-5.20474889637625E-17));
#10125=CARTESIAN_POINT('Origin',(0.,0.45,0.));
#10126=CARTESIAN_POINT('',(-0.4,0.475,-4.89858719658941E-17));
#10127=CARTESIAN_POINT('Origin',(0.,0.24,0.));
#10128=CARTESIAN_POINT('',(-0.425,0.0299999999999998,-5.20474889637625E-17));
#10129=CARTESIAN_POINT('Origin',(0.,0.0299999999999998,0.));
#10130=CARTESIAN_POINT('',(-0.425,0.24,-5.20474889637625E-17));
#10131=CARTESIAN_POINT('Origin',(0.,0.0150000000000001,0.));
#10132=CARTESIAN_POINT('',(-0.395,4.85722573273506E-17,-4.83735485663204E-17));
#10133=CARTESIAN_POINT('Origin',(0.,0.,0.));
#10134=CARTESIAN_POINT('',(-0.41,0.0150000000000001,-5.02105187650415E-17));
#10135=CARTESIAN_POINT('Origin',(0.27,0.,0.));
#10136=CARTESIAN_POINT('',(-0.27,0.,-3.30654635769785E-17));
#10137=CARTESIAN_POINT('Origin',(0.,0.,0.));
#10138=CARTESIAN_POINT('Origin',(0.,-0.02,0.));
#10139=CARTESIAN_POINT('',(-0.24505,-0.0498999999999999,3.00099698131059E-17));
#10140=CARTESIAN_POINT('Origin',(0.,-0.0498999999999999,0.));
#10141=CARTESIAN_POINT('',(-0.26,-0.02,-3.18408167778312E-17));
#10142=CARTESIAN_POINT('Origin',(0.,-0.995,0.));
#10143=CARTESIAN_POINT('',(-0.24505,-0.995,-3.00099698131059E-17));
#10144=CARTESIAN_POINT('',(0.,0.,0.));
#10145=CARTESIAN_POINT('Origin',(0.144337567297406,-0.6,-0.25));
#10146=CARTESIAN_POINT('',(0.288675134594813,-0.6,0.));
#10147=CARTESIAN_POINT('',(0.144337567297406,-0.6,-0.25));
#10148=CARTESIAN_POINT('',(0.288675134594813,-0.6,0.));
#10149=CARTESIAN_POINT('',(0.144337567297406,-0.96,-0.25));
#10150=CARTESIAN_POINT('',(0.144337567297406,-0.6,-0.25));
#10151=CARTESIAN_POINT('',(0.288675134594813,-0.96,0.));
#10152=CARTESIAN_POINT('',(0.288675134594813,-0.96,0.));
#10153=CARTESIAN_POINT('',(0.288675134594813,-0.6,0.));
#10154=CARTESIAN_POINT('Origin',(-0.144337567297406,-0.6,-0.25));
#10155=CARTESIAN_POINT('',(-0.144337567297406,-0.6,-0.25));
#10156=CARTESIAN_POINT('',(0.144337567297406,-0.6,-0.25));
#10157=CARTESIAN_POINT('',(-0.144337567297406,-0.96,-0.25));
#10158=CARTESIAN_POINT('',(-0.144337567297406,-0.6,-0.25));
#10159=CARTESIAN_POINT('',(0.144337567297406,-0.96,-0.25));
#10160=CARTESIAN_POINT('Origin',(-0.288675134594813,-0.6,-8.32667268468867E-17));
#10161=CARTESIAN_POINT('',(-0.288675134594813,-0.6,-3.53525079574969E-17));
#10162=CARTESIAN_POINT('',(-0.144337567297406,-0.6,-0.25));
#10163=CARTESIAN_POINT('',(-0.288675134594813,-0.96,-5.55111512312578E-17));
#10164=CARTESIAN_POINT('',(-0.288675134594813,-0.6,-3.53525079574969E-17));
#10165=CARTESIAN_POINT('',(-0.144337567297406,-0.96,-0.25));
#10166=CARTESIAN_POINT('Origin',(-0.144337567297407,-0.6,0.25));
#10167=CARTESIAN_POINT('',(-0.144337567297407,-0.6,0.25));
#10168=CARTESIAN_POINT('',(-0.288675134594813,-0.6,-3.53525079574969E-17));
#10169=CARTESIAN_POINT('',(-0.144337567297407,-0.96,0.25));
#10170=CARTESIAN_POINT('',(-0.144337567297407,-0.6,0.25));
#10171=CARTESIAN_POINT('',(-0.288675134594813,-0.96,-3.53525079574969E-17));
#10172=CARTESIAN_POINT('Origin',(0.144337567297406,-0.6,0.25));
#10173=CARTESIAN_POINT('',(0.144337567297406,-0.6,0.25));
#10174=CARTESIAN_POINT('',(-0.144337567297407,-0.6,0.25));
#10175=CARTESIAN_POINT('',(0.144337567297406,-0.96,0.25));
#10176=CARTESIAN_POINT('',(0.144337567297406,-0.6,0.25));
#10177=CARTESIAN_POINT('',(-0.144337567297407,-0.96,0.25));
#10178=CARTESIAN_POINT('Origin',(0.288675134594813,-0.6,0.));
#10179=CARTESIAN_POINT('',(0.144337567297406,-0.6,0.25));
#10180=CARTESIAN_POINT('',(0.144337567297406,-0.96,0.25));
#10181=CARTESIAN_POINT('Origin',(0.,-0.6,0.));
#10182=CARTESIAN_POINT('Origin',(0.,-0.96,0.));
#10183=CARTESIAN_POINT('Origin',(0.,-1.8,0.));
#10184=CARTESIAN_POINT('',(-0.2942,-1.8,3.60291088309151E-17));
#10185=CARTESIAN_POINT('Origin',(0.,-1.8,0.));
#10186=CARTESIAN_POINT('Origin',(0.45,0.6,0.));
#10187=CARTESIAN_POINT('',(-0.45,0.6,-5.51091059616309E-17));
#10188=CARTESIAN_POINT('Origin',(0.,0.6,0.));
#10189=CARTESIAN_POINT('Origin',(0.,0.575,0.));
#10190=CARTESIAN_POINT('',(-0.5,0.55,-6.12323399573677E-17));
#10191=CARTESIAN_POINT('Origin',(0.,0.55,0.));
#10192=CARTESIAN_POINT('',(-0.475,0.575,-5.81707229594993E-17));
#10193=CARTESIAN_POINT('Origin',(0.,0.29,0.));
#10194=CARTESIAN_POINT('',(-0.5,0.0299999999999998,-6.12323399573677E-17));
#10195=CARTESIAN_POINT('Origin',(0.,0.0299999999999998,0.));
#10196=CARTESIAN_POINT('',(-0.5,0.29,-6.12323399573677E-17));
#10197=CARTESIAN_POINT('Origin',(0.,0.0150000000000001,0.));
#10198=CARTESIAN_POINT('',(-0.47,7.11236625150491E-17,-5.75583995599256E-17));
#10199=CARTESIAN_POINT('Origin',(0.,0.,0.));
#10200=CARTESIAN_POINT('',(-0.485,0.0150000000000001,-5.93953697586466E-17));
#10201=CARTESIAN_POINT('Origin',(0.32,0.,0.));
#10202=CARTESIAN_POINT('',(-0.32,-6.93889390390723E-18,-3.91886975727153E-17));
#10203=CARTESIAN_POINT('Origin',(0.,0.,0.));
#10204=CARTESIAN_POINT('Origin',(0.,-0.02,0.));
#10205=CARTESIAN_POINT('',(-0.2942,-0.0515999999999999,3.60291088309151E-17));
#10206=CARTESIAN_POINT('Origin',(0.,-0.0515999999999999,0.));
#10207=CARTESIAN_POINT('',(-0.31,-0.02,-3.7964050773568E-17));
#10208=CARTESIAN_POINT('Origin',(0.,-1.24,0.));
#10209=CARTESIAN_POINT('',(-0.2942,-1.24,-3.60291088309151E-17));
#10210=CARTESIAN_POINT('',(0.,0.,0.));
#10211=CARTESIAN_POINT('',(0.,0.,0.));
#10212=CARTESIAN_POINT('Origin',(0.,0.,0.));
#10213=CARTESIAN_POINT('',(-2.05,-1.665,2.51052593825207E-16));
#10214=CARTESIAN_POINT('Origin',(0.,-1.665,0.));
#10215=CARTESIAN_POINT('',(-2.05,-1.14891252930761,-2.51052593825207E-16));
#10216=CARTESIAN_POINT('',(-2.05,0.,2.51052593825207E-16));
#10217=CARTESIAN_POINT('Origin',(0.,-1.14891252930761,0.));
#10218=CARTESIAN_POINT('Origin',(0.,0.,0.));
#10219=CARTESIAN_POINT('',(-2.05,1.14891252930761,2.51052593825207E-16));
#10220=CARTESIAN_POINT('Origin',(0.,1.14891252930761,0.));
#10221=CARTESIAN_POINT('',(-2.05,1.665,-2.51052593825207E-16));
#10222=CARTESIAN_POINT('',(-2.05,0.,2.51052593825207E-16));
#10223=CARTESIAN_POINT('Origin',(0.,1.665,0.));
#10224=CARTESIAN_POINT('Origin',(0.,0.,0.));
#10225=CARTESIAN_POINT('',(-1.43895998899814E-16,-1.76221774462768E-32,
-2.35));
#10226=CARTESIAN_POINT('',(-1.43895998899814E-16,-1.76221774462768E-32,
2.35));
#10227=CARTESIAN_POINT('Origin',(0.,0.,0.));
#10228=CARTESIAN_POINT('Origin',(0.,0.,0.));
#10229=CARTESIAN_POINT('',(-3.,-0.5,3.67394039744206E-16));
#10230=CARTESIAN_POINT('Origin',(0.,-0.5,0.));
#10231=CARTESIAN_POINT('',(-3.,-1.665,3.67394039744206E-16));
#10232=CARTESIAN_POINT('',(-3.,0.,3.67394039744206E-16));
#10233=CARTESIAN_POINT('Origin',(0.,-1.665,0.));
#10234=CARTESIAN_POINT('Origin',(0.,0.,0.));
#10235=CARTESIAN_POINT('',(-3.,1.665,3.67394039744206E-16));
#10236=CARTESIAN_POINT('Origin',(0.,1.665,0.));
#10237=CARTESIAN_POINT('',(-3.,0.5,-3.67394039744206E-16));
#10238=CARTESIAN_POINT('',(-3.,0.,3.67394039744206E-16));
#10239=CARTESIAN_POINT('Origin',(0.,0.5,0.));
#10240=CARTESIAN_POINT('Origin',(0.,-1.665,0.));
#10241=CARTESIAN_POINT('Origin',(0.,1.665,0.));
#10242=CARTESIAN_POINT('Origin',(3.2,0.,3.2));
#10243=CARTESIAN_POINT('',(2.6,-0.5,3.2));
#10244=CARTESIAN_POINT('Origin',(3.2,-0.5,3.2));
#10245=CARTESIAN_POINT('',(2.6,0.5,3.2));
#10246=CARTESIAN_POINT('',(2.6,0.,3.2));
#10247=CARTESIAN_POINT('Origin',(3.2,0.5,3.2));
#10248=CARTESIAN_POINT('Origin',(-3.2,0.,-3.2));
#10249=CARTESIAN_POINT('',(-3.8,-0.5,-3.2));
#10250=CARTESIAN_POINT('Origin',(-3.2,-0.5,-3.2));
#10251=CARTESIAN_POINT('',(-3.8,0.5,-3.2));
#10252=CARTESIAN_POINT('',(-3.8,0.,-3.2));
#10253=CARTESIAN_POINT('Origin',(-3.2,0.5,-3.2));
#10254=CARTESIAN_POINT('Origin',(-3.2,0.,3.2));
#10255=CARTESIAN_POINT('',(-3.8,-0.5,3.2));
#10256=CARTESIAN_POINT('Origin',(-3.2,-0.5,3.2));
#10257=CARTESIAN_POINT('',(-3.8,0.5,3.2));
#10258=CARTESIAN_POINT('',(-3.8,0.,3.2));
#10259=CARTESIAN_POINT('Origin',(-3.2,0.5,3.2));
#10260=CARTESIAN_POINT('Origin',(3.2,0.,-3.2));
#10261=CARTESIAN_POINT('',(2.6,-0.5,-3.2));
#10262=CARTESIAN_POINT('Origin',(3.2,-0.5,-3.2));
#10263=CARTESIAN_POINT('',(2.6,0.5,-3.2));
#10264=CARTESIAN_POINT('',(2.6,0.,-3.2));
#10265=CARTESIAN_POINT('Origin',(3.2,0.5,-3.2));
#10266=CARTESIAN_POINT('Origin',(-4.3,-0.5,-3.3));
#10267=CARTESIAN_POINT('',(-4.3,-0.5,-3.3));
#10268=CARTESIAN_POINT('',(-4.3,-0.5,3.3));
#10269=CARTESIAN_POINT('',(-4.3,-0.5,-3.3));
#10270=CARTESIAN_POINT('',(-4.3,0.5,3.3));
#10271=CARTESIAN_POINT('',(-4.3,-0.5,3.3));
#10272=CARTESIAN_POINT('',(-4.3,0.5,-3.3));
#10273=CARTESIAN_POINT('',(-4.3,0.5,-3.3));
#10274=CARTESIAN_POINT('',(-4.3,-0.5,-3.3));
#10275=CARTESIAN_POINT('Origin',(-3.3,-0.5,-4.3));
#10276=CARTESIAN_POINT('',(-3.3,-0.5,-4.3));
#10277=CARTESIAN_POINT('',(-3.3,-0.5,-4.3));
#10278=CARTESIAN_POINT('',(-3.3,0.5,-4.3));
#10279=CARTESIAN_POINT('',(-3.3,0.5,-4.3));
#10280=CARTESIAN_POINT('',(-3.3,-0.5,-4.3));
#10281=CARTESIAN_POINT('Origin',(3.3,-0.5,-4.3));
#10282=CARTESIAN_POINT('',(3.3,-0.5,-4.3));
#10283=CARTESIAN_POINT('',(3.3,-0.5,-4.3));
#10284=CARTESIAN_POINT('',(3.3,0.5,-4.3));
#10285=CARTESIAN_POINT('',(3.3,0.5,-4.3));
#10286=CARTESIAN_POINT('',(3.3,-0.5,-4.3));
#10287=CARTESIAN_POINT('Origin',(4.3,-0.5,-3.3));
#10288=CARTESIAN_POINT('',(4.3,-0.5,-3.3));
#10289=CARTESIAN_POINT('',(4.3,-0.5,-3.3));
#10290=CARTESIAN_POINT('',(4.3,0.5,-3.3));
#10291=CARTESIAN_POINT('',(4.3,0.5,-3.3));
#10292=CARTESIAN_POINT('',(4.3,-0.5,-3.3));
#10293=CARTESIAN_POINT('Origin',(4.3,-0.5,3.3));
#10294=CARTESIAN_POINT('',(4.3,-0.5,3.3));
#10295=CARTESIAN_POINT('',(4.3,-0.5,3.3));
#10296=CARTESIAN_POINT('',(4.3,0.5,3.3));
#10297=CARTESIAN_POINT('',(4.3,0.5,3.3));
#10298=CARTESIAN_POINT('',(4.3,-0.5,3.3));
#10299=CARTESIAN_POINT('Origin',(3.3,-0.5,4.3));
#10300=CARTESIAN_POINT('',(3.3,-0.5,4.3));
#10301=CARTESIAN_POINT('',(3.3,-0.5,4.3));
#10302=CARTESIAN_POINT('',(3.3,0.5,4.3));
#10303=CARTESIAN_POINT('',(3.3,0.5,4.3));
#10304=CARTESIAN_POINT('',(3.3,-0.5,4.3));
#10305=CARTESIAN_POINT('Origin',(-3.3,-0.5,4.3));
#10306=CARTESIAN_POINT('',(-3.3,-0.5,4.3));
#10307=CARTESIAN_POINT('',(-3.3,-0.5,4.3));
#10308=CARTESIAN_POINT('',(-3.3,0.5,4.3));
#10309=CARTESIAN_POINT('',(-3.3,0.5,4.3));
#10310=CARTESIAN_POINT('',(-3.3,-0.5,4.3));
#10311=CARTESIAN_POINT('Origin',(-4.3,-0.5,3.3));
#10312=CARTESIAN_POINT('',(-4.3,-0.5,3.3));
#10313=CARTESIAN_POINT('',(-4.3,0.5,3.3));
#10314=CARTESIAN_POINT('Origin',(0.,0.5,0.));
#10315=CARTESIAN_POINT('Origin',(0.,-0.5,0.));
#10316=CARTESIAN_POINT('',(0.,0.,0.));
#10317=CARTESIAN_POINT('Origin',(0.,0.,0.));
#10318=CARTESIAN_POINT('',(-1.8,-0.85,-2.20436423846524E-16));
#10319=CARTESIAN_POINT('Origin',(0.,-0.85,0.));
#10320=CARTESIAN_POINT('',(-1.8,0.85,-2.20436423846524E-16));
#10321=CARTESIAN_POINT('',(-1.8,0.,-2.20436423846524E-16));
#10322=CARTESIAN_POINT('Origin',(0.,0.85,0.));
#10323=CARTESIAN_POINT('Origin',(2.19089023002066,0.85,0.));
#10324=CARTESIAN_POINT('',(2.19089023002066,0.85,0.));
#10325=CARTESIAN_POINT('Origin',(0.,0.85,0.));
#10326=CARTESIAN_POINT('Origin',(3.99680288865056E-15,0.,0.));
#10327=CARTESIAN_POINT('',(3.85290688975075E-15,-1.76221774462768E-32,2.35));
#10328=CARTESIAN_POINT('',(3.85290688975075E-15,-1.76221774462768E-32,-2.35));
#10329=CARTESIAN_POINT('Origin',(3.99680288865056E-15,0.,0.));
#10330=CARTESIAN_POINT('',(2.19089023002066,-0.85,0.));
#10331=CARTESIAN_POINT('Origin',(0.,-0.85,0.));
#10332=CARTESIAN_POINT('Origin',(1.8,-0.85,0.));
#10333=CARTESIAN_POINT('Origin',(0.,1.55,0.));
#10334=CARTESIAN_POINT('',(1.42894191624432,1.8,0.825000000000001));
#10335=CARTESIAN_POINT('',(1.53744468918255,1.55,0.598968970568896));
#10336=CARTESIAN_POINT('Ctrl Pts',(1.42894191624432,1.8,0.825000000000001));
#10337=CARTESIAN_POINT('Ctrl Pts',(1.44466308895875,1.8,0.797770130104052));
#10338=CARTESIAN_POINT('Ctrl Pts',(1.46055812562105,1.79370633789704,0.768258557763732));
#10339=CARTESIAN_POINT('Ctrl Pts',(1.48824888379079,1.76817777258318,0.713138492740816));
#10340=CARTESIAN_POINT('Ctrl Pts',(1.50008999307766,1.74894552961493,0.687551581002689));
#10341=CARTESIAN_POINT('Ctrl Pts',(1.51812136280714,1.70460745840382,0.646764802471699));
#10342=CARTESIAN_POINT('Ctrl Pts',(1.52552758004446,1.67652816181843,0.628833667319578));
#10343=CARTESIAN_POINT('Ctrl Pts',(1.53516661651472,1.61494799959182,0.604921184808251));
#10344=CARTESIAN_POINT('Ctrl Pts',(1.53744468918255,1.58144291640553,0.598968970568896));
#10345=CARTESIAN_POINT('Ctrl Pts',(1.53744468918255,1.55,0.598968970568896));
#10346=CARTESIAN_POINT('',(1.42894191624432,1.3,0.825000000000001));
#10347=CARTESIAN_POINT('Ctrl Pts',(1.42894191624432,1.3,0.825000000000001));
#10348=CARTESIAN_POINT('Ctrl Pts',(1.4132207435299,1.3,0.852229869895949));
#10349=CARTESIAN_POINT('Ctrl Pts',(1.39561049050871,1.30629366210296,0.880751161609749));
#10350=CARTESIAN_POINT('Ctrl Pts',(1.36172049302549,1.33182222741682,0.932292094146256));
#10351=CARTESIAN_POINT('Ctrl Pts',(1.34548213209931,1.35105447038507,0.955340251466734));
#10352=CARTESIAN_POINT('Ctrl Pts',(1.31917543061769,1.39539254159618,0.99134926498299));
#10353=CARTESIAN_POINT('Ctrl Pts',(1.30734972067592,1.42347183818157,1.00672880483252));
#10354=CARTESIAN_POINT('Ctrl Pts',(1.29146042158868,1.48505200040818,1.02703269653942));
#10355=CARTESIAN_POINT('Ctrl Pts',(1.28744468918255,1.51855708359447,1.03198167246111));
#10356=CARTESIAN_POINT('Ctrl Pts',(1.28744468918255,1.58144291640553,1.03198167246111));
#10357=CARTESIAN_POINT('Ctrl Pts',(1.29146042158868,1.61494799959182,1.02703269653942));
#10358=CARTESIAN_POINT('Ctrl Pts',(1.30734972067592,1.67652816181843,1.00672880483252));
#10359=CARTESIAN_POINT('Ctrl Pts',(1.31917543061769,1.70460745840382,0.991349264982991));
#10360=CARTESIAN_POINT('Ctrl Pts',(1.34548213209931,1.74894552961493,0.955340251466735));
#10361=CARTESIAN_POINT('Ctrl Pts',(1.36172049302549,1.76817777258318,0.932292094146256));
#10362=CARTESIAN_POINT('Ctrl Pts',(1.39561049050871,1.79370633789704,0.880751161609749));
#10363=CARTESIAN_POINT('Ctrl Pts',(1.4132207435299,1.8,0.85222986989595));
#10364=CARTESIAN_POINT('Ctrl Pts',(1.42894191624432,1.8,0.825000000000001));
#10365=CARTESIAN_POINT('Ctrl Pts',(1.53744468918255,1.55,0.598968970568896));
#10366=CARTESIAN_POINT('Ctrl Pts',(1.53744468918255,1.51855708359447,0.598968970568896));
#10367=CARTESIAN_POINT('Ctrl Pts',(1.53516661651472,1.48505200040818,0.60492118480825));
#10368=CARTESIAN_POINT('Ctrl Pts',(1.52552758004446,1.42347183818157,0.628833667319578));
#10369=CARTESIAN_POINT('Ctrl Pts',(1.51812136280714,1.39539254159618,0.646764802471699));
#10370=CARTESIAN_POINT('Ctrl Pts',(1.50008999307766,1.35105447038507,0.687551581002689));
#10371=CARTESIAN_POINT('Ctrl Pts',(1.48824888379079,1.33182222741682,0.713138492740816));
#10372=CARTESIAN_POINT('Ctrl Pts',(1.46055812562105,1.30629366210296,0.768258557763732));
#10373=CARTESIAN_POINT('Ctrl Pts',(1.44466308895875,1.3,0.797770130104052));
#10374=CARTESIAN_POINT('Ctrl Pts',(1.42894191624432,1.3,0.825000000000001));
#10375=CARTESIAN_POINT('',(0.59736109069228,1.55,0.0562114519197835));
#10376=CARTESIAN_POINT('',(0.125,1.55,-0.21650635094611));
#10377=CARTESIAN_POINT('Ctrl Pts',(0.59736109069228,1.55,0.0562114519197835));
#10378=CARTESIAN_POINT('Ctrl Pts',(0.59736109069228,1.58183602855499,0.0562114519197835));
#10379=CARTESIAN_POINT('Ctrl Pts',(0.596809586309859,1.61548166177648,0.0633319361811907));
#10380=CARTESIAN_POINT('Ctrl Pts',(0.593243052195919,1.67693412158597,0.0908585874761106));
#10381=CARTESIAN_POINT('Ctrl Pts',(0.590063593315144,1.70478184753241,0.111151766652641));
#10382=CARTESIAN_POINT('Ctrl Pts',(0.579820497891285,1.74874496453875,0.15600214762839));
#10383=CARTESIAN_POINT('Ctrl Pts',(0.572042315803119,1.76792916820474,0.183678633836535));
#10384=CARTESIAN_POINT('Ctrl Pts',(0.549947124580676,1.79356669468566,0.241926459727039));
#10385=CARTESIAN_POINT('Ctrl Pts',(0.53551402125728,1.8,0.27246250701687));
#10386=CARTESIAN_POINT('Ctrl Pts',(0.503716463284046,1.8,0.32753749298313));
#10387=CARTESIAN_POINT('Ctrl Pts',(0.484488022261586,1.79356669468566,0.355304950761552));
#10388=CARTESIAN_POINT('Ctrl Pts',(0.445091520936419,1.76792916820474,0.403563860606914));
#10389=CARTESIAN_POINT('Ctrl Pts',(0.425012071836758,1.74874496453875,0.4241382069946));
#10390=CARTESIAN_POINT('Ctrl Pts',(0.391292050254278,1.70478184753241,0.455434178332924));
#10391=CARTESIAN_POINT('Ctrl Pts',(0.375307371004241,1.67693412158597,0.468334260082228));
#10392=CARTESIAN_POINT('Ctrl Pts',(0.353251858758695,1.61548166177647,0.485186294875824));
#10393=CARTESIAN_POINT('Ctrl Pts',(0.347361090692279,1.58183602855499,0.489224153812003));
#10394=CARTESIAN_POINT('Ctrl Pts',(0.347361090692279,1.51816397144501,0.489224153812003));
#10395=CARTESIAN_POINT('Ctrl Pts',(0.353251858758695,1.48451833822352,0.485186294875824));
#10396=CARTESIAN_POINT('Ctrl Pts',(0.375307371004241,1.42306587841403,0.468334260082228));
#10397=CARTESIAN_POINT('Ctrl Pts',(0.391292050254278,1.39521815246759,0.455434178332924));
#10398=CARTESIAN_POINT('Ctrl Pts',(0.425012071836758,1.35125503546125,0.4241382069946));
#10399=CARTESIAN_POINT('Ctrl Pts',(0.445091520936418,1.33207083179526,0.403563860606914));
#10400=CARTESIAN_POINT('Ctrl Pts',(0.484488022261586,1.30643330531434,0.355304950761552));
#10401=CARTESIAN_POINT('Ctrl Pts',(0.503716463284046,1.3,0.32753749298313));
#10402=CARTESIAN_POINT('Ctrl Pts',(0.53551402125728,1.3,0.27246250701687));
#10403=CARTESIAN_POINT('Ctrl Pts',(0.549947124580676,1.30643330531434,0.241926459727039));
#10404=CARTESIAN_POINT('Ctrl Pts',(0.572042315803119,1.33207083179526,0.183678633836535));
#10405=CARTESIAN_POINT('Ctrl Pts',(0.579820497891285,1.35125503546125,0.15600214762839));
#10406=CARTESIAN_POINT('Ctrl Pts',(0.590063593315144,1.39521815246759,0.111151766652641));
#10407=CARTESIAN_POINT('Ctrl Pts',(0.593243052195919,1.42306587841403,0.0908585874761105));
#10408=CARTESIAN_POINT('Ctrl Pts',(0.596809586309859,1.48451833822352,0.0633319361811906));
#10409=CARTESIAN_POINT('Ctrl Pts',(0.59736109069228,1.51816397144501,0.0562114519197835));
#10410=CARTESIAN_POINT('Ctrl Pts',(0.59736109069228,1.55,0.0562114519197835));
#10411=CARTESIAN_POINT('Origin',(0.,1.55,0.));
#10412=CARTESIAN_POINT('',(-0.347361090692279,1.55,-0.489224153812003));
#10413=CARTESIAN_POINT('Ctrl Pts',(-0.347361090692279,1.55,-0.489224153812003));
#10414=CARTESIAN_POINT('Ctrl Pts',(-0.347361090692279,1.51816397144501,
-0.489224153812003));
#10415=CARTESIAN_POINT('Ctrl Pts',(-0.353251858758695,1.48451833822352,
-0.485186294875824));
#10416=CARTESIAN_POINT('Ctrl Pts',(-0.375307371004241,1.42306587841403,
-0.468334260082228));
#10417=CARTESIAN_POINT('Ctrl Pts',(-0.391292050254278,1.39521815246759,
-0.455434178332924));
#10418=CARTESIAN_POINT('Ctrl Pts',(-0.425012071836758,1.35125503546125,
-0.4241382069946));
#10419=CARTESIAN_POINT('Ctrl Pts',(-0.445091520936419,1.33207083179526,
-0.403563860606914));
#10420=CARTESIAN_POINT('Ctrl Pts',(-0.484488022261586,1.30643330531434,
-0.355304950761552));
#10421=CARTESIAN_POINT('Ctrl Pts',(-0.503716463284046,1.3,-0.32753749298313));
#10422=CARTESIAN_POINT('Ctrl Pts',(-0.53551402125728,1.3,-0.27246250701687));
#10423=CARTESIAN_POINT('Ctrl Pts',(-0.549947124580676,1.30643330531434,
-0.241926459727039));
#10424=CARTESIAN_POINT('Ctrl Pts',(-0.572042315803119,1.33207083179526,
-0.183678633836535));
#10425=CARTESIAN_POINT('Ctrl Pts',(-0.579820497891285,1.35125503546125,
-0.15600214762839));
#10426=CARTESIAN_POINT('Ctrl Pts',(-0.590063593315144,1.39521815246759,
-0.111151766652641));
#10427=CARTESIAN_POINT('Ctrl Pts',(-0.593243052195918,1.42306587841403,
-0.0908585874761106));
#10428=CARTESIAN_POINT('Ctrl Pts',(-0.596809586309859,1.48451833822352,
-0.0633319361811906));
#10429=CARTESIAN_POINT('Ctrl Pts',(-0.597361090692279,1.51816397144501,
-0.0562114519197835));
#10430=CARTESIAN_POINT('Ctrl Pts',(-0.597361090692279,1.58183602855499,
-0.0562114519197835));
#10431=CARTESIAN_POINT('Ctrl Pts',(-0.596809586309859,1.61548166177647,
-0.0633319361811905));
#10432=CARTESIAN_POINT('Ctrl Pts',(-0.593243052195918,1.67693412158597,
-0.0908585874761104));
#10433=CARTESIAN_POINT('Ctrl Pts',(-0.590063593315144,1.70478184753241,
-0.111151766652641));
#10434=CARTESIAN_POINT('Ctrl Pts',(-0.579820497891285,1.74874496453875,
-0.15600214762839));
#10435=CARTESIAN_POINT('Ctrl Pts',(-0.572042315803118,1.76792916820474,
-0.183678633836535));
#10436=CARTESIAN_POINT('Ctrl Pts',(-0.549947124580676,1.79356669468566,
-0.241926459727039));
#10437=CARTESIAN_POINT('Ctrl Pts',(-0.53551402125728,1.8,-0.27246250701687));
#10438=CARTESIAN_POINT('Ctrl Pts',(-0.503716463284046,1.8,-0.32753749298313));
#10439=CARTESIAN_POINT('Ctrl Pts',(-0.484488022261586,1.79356669468566,
-0.355304950761552));
#10440=CARTESIAN_POINT('Ctrl Pts',(-0.445091520936419,1.76792916820474,
-0.403563860606914));
#10441=CARTESIAN_POINT('Ctrl Pts',(-0.425012071836758,1.74874496453875,
-0.4241382069946));
#10442=CARTESIAN_POINT('Ctrl Pts',(-0.391292050254278,1.70478184753241,
-0.455434178332924));
#10443=CARTESIAN_POINT('Ctrl Pts',(-0.375307371004241,1.67693412158597,
-0.468334260082228));
#10444=CARTESIAN_POINT('Ctrl Pts',(-0.353251858758695,1.61548166177648,
-0.485186294875824));
#10445=CARTESIAN_POINT('Ctrl Pts',(-0.347361090692279,1.58183602855499,
-0.489224153812003));
#10446=CARTESIAN_POINT('Ctrl Pts',(-0.347361090692279,1.55,-0.489224153812003));
#10447=CARTESIAN_POINT('',(-1.28744468918255,1.55,-1.03198167246111));
#10448=CARTESIAN_POINT('',(0.125,1.55,-0.21650635094611));
#10449=CARTESIAN_POINT('',(-1.42894191624432,1.3,-0.825000000000001));
#10450=CARTESIAN_POINT('Ctrl Pts',(-1.42894191624432,1.3,-0.825000000000001));
#10451=CARTESIAN_POINT('Ctrl Pts',(-1.4132207435299,1.3,-0.852229869895949));
#10452=CARTESIAN_POINT('Ctrl Pts',(-1.39561049050871,1.30629366210296,-0.880751161609749));
#10453=CARTESIAN_POINT('Ctrl Pts',(-1.36172049302549,1.33182222741682,-0.932292094146256));
#10454=CARTESIAN_POINT('Ctrl Pts',(-1.34548213209931,1.35105447038507,-0.955340251466735));
#10455=CARTESIAN_POINT('Ctrl Pts',(-1.31917543061769,1.39539254159618,-0.991349264982991));
#10456=CARTESIAN_POINT('Ctrl Pts',(-1.30734972067592,1.42347183818157,-1.00672880483252));
#10457=CARTESIAN_POINT('Ctrl Pts',(-1.29146042158868,1.48505200040818,-1.02703269653942));
#10458=CARTESIAN_POINT('Ctrl Pts',(-1.28744468918255,1.51855708359447,-1.03198167246111));
#10459=CARTESIAN_POINT('Ctrl Pts',(-1.28744468918255,1.55,-1.03198167246111));
#10460=CARTESIAN_POINT('',(-1.42894191624432,1.8,-0.825000000000001));
#10461=CARTESIAN_POINT('Ctrl Pts',(-1.42894191624432,1.8,-0.825000000000001));
#10462=CARTESIAN_POINT('Ctrl Pts',(-1.44466308895875,1.8,-0.797770130104052));
#10463=CARTESIAN_POINT('Ctrl Pts',(-1.46055812562105,1.79370633789704,-0.768258557763732));
#10464=CARTESIAN_POINT('Ctrl Pts',(-1.48824888379079,1.76817777258318,-0.713138492740816));
#10465=CARTESIAN_POINT('Ctrl Pts',(-1.50008999307766,1.74894552961493,-0.687551581002689));
#10466=CARTESIAN_POINT('Ctrl Pts',(-1.51812136280714,1.70460745840382,-0.646764802471699));
#10467=CARTESIAN_POINT('Ctrl Pts',(-1.52552758004446,1.67652816181843,-0.628833667319578));
#10468=CARTESIAN_POINT('Ctrl Pts',(-1.53516661651472,1.61494799959182,-0.60492118480825));
#10469=CARTESIAN_POINT('Ctrl Pts',(-1.53744468918255,1.58144291640553,-0.598968970568896));
#10470=CARTESIAN_POINT('Ctrl Pts',(-1.53744468918255,1.51855708359447,-0.598968970568896));
#10471=CARTESIAN_POINT('Ctrl Pts',(-1.53516661651472,1.48505200040818,-0.60492118480825));
#10472=CARTESIAN_POINT('Ctrl Pts',(-1.52552758004446,1.42347183818157,-0.628833667319578));
#10473=CARTESIAN_POINT('Ctrl Pts',(-1.51812136280714,1.39539254159618,-0.646764802471699));
#10474=CARTESIAN_POINT('Ctrl Pts',(-1.50008999307766,1.35105447038507,-0.687551581002689));
#10475=CARTESIAN_POINT('Ctrl Pts',(-1.48824888379079,1.33182222741682,-0.713138492740816));
#10476=CARTESIAN_POINT('Ctrl Pts',(-1.46055812562105,1.30629366210296,-0.768258557763732));
#10477=CARTESIAN_POINT('Ctrl Pts',(-1.44466308895875,1.3,-0.797770130104052));
#10478=CARTESIAN_POINT('Ctrl Pts',(-1.42894191624432,1.3,-0.825000000000001));
#10479=CARTESIAN_POINT('Ctrl Pts',(-1.28744468918255,1.55,-1.03198167246111));
#10480=CARTESIAN_POINT('Ctrl Pts',(-1.28744468918255,1.58144291640553,-1.03198167246111));
#10481=CARTESIAN_POINT('Ctrl Pts',(-1.29146042158868,1.61494799959182,-1.02703269653942));
#10482=CARTESIAN_POINT('Ctrl Pts',(-1.30734972067592,1.67652816181843,-1.00672880483252));
#10483=CARTESIAN_POINT('Ctrl Pts',(-1.31917543061769,1.70460745840382,-0.991349264982991));
#10484=CARTESIAN_POINT('Ctrl Pts',(-1.34548213209931,1.74894552961493,-0.955340251466734));
#10485=CARTESIAN_POINT('Ctrl Pts',(-1.36172049302549,1.76817777258318,-0.932292094146256));
#10486=CARTESIAN_POINT('Ctrl Pts',(-1.39561049050871,1.79370633789704,-0.880751161609749));
#10487=CARTESIAN_POINT('Ctrl Pts',(-1.4132207435299,1.8,-0.852229869895949));
#10488=CARTESIAN_POINT('Ctrl Pts',(-1.42894191624432,1.8,-0.825000000000001));
#10489=CARTESIAN_POINT('Origin',(0.,1.55,0.));
#10490=CARTESIAN_POINT('',(-1.65,0.85,-2.02066721859313E-16));
#10491=CARTESIAN_POINT('Origin',(0.,0.85,0.));
#10492=CARTESIAN_POINT('',(-1.65,2.25,-2.02066721859313E-16));
#10493=CARTESIAN_POINT('',(-1.65,1.55,-2.02066721859313E-16));
#10494=CARTESIAN_POINT('Origin',(0.,2.25,0.));
#10495=CARTESIAN_POINT('',(-1.42894191624432,1.3,0.825));
#10496=CARTESIAN_POINT('',(-1.42894191624432,1.8,0.825));
#10497=CARTESIAN_POINT('Ctrl Pts',(-1.42894191624432,1.3,0.825));
#10498=CARTESIAN_POINT('Ctrl Pts',(-1.44466308895875,1.3,0.797770130104051));
#10499=CARTESIAN_POINT('Ctrl Pts',(-1.46055812562105,1.30629366210296,0.768258557763731));
#10500=CARTESIAN_POINT('Ctrl Pts',(-1.48824888379079,1.33182222741682,0.713138492740815));
#10501=CARTESIAN_POINT('Ctrl Pts',(-1.50008999307766,1.35105447038507,0.687551581002688));
#10502=CARTESIAN_POINT('Ctrl Pts',(-1.51812136280714,1.39539254159618,0.646764802471698));
#10503=CARTESIAN_POINT('Ctrl Pts',(-1.52552758004446,1.42347183818157,0.628833667319577));
#10504=CARTESIAN_POINT('Ctrl Pts',(-1.53516661651472,1.48505200040818,0.604921184808249));
#10505=CARTESIAN_POINT('Ctrl Pts',(-1.53744468918255,1.51855708359447,0.598968970568895));
#10506=CARTESIAN_POINT('Ctrl Pts',(-1.53744468918255,1.58144291640553,0.598968970568895));
#10507=CARTESIAN_POINT('Ctrl Pts',(-1.53516661651472,1.61494799959182,0.604921184808249));
#10508=CARTESIAN_POINT('Ctrl Pts',(-1.52552758004446,1.67652816181843,0.628833667319577));
#10509=CARTESIAN_POINT('Ctrl Pts',(-1.51812136280714,1.70460745840382,0.646764802471698));
#10510=CARTESIAN_POINT('Ctrl Pts',(-1.50008999307766,1.74894552961493,0.687551581002688));
#10511=CARTESIAN_POINT('Ctrl Pts',(-1.48824888379079,1.76817777258318,0.713138492740815));
#10512=CARTESIAN_POINT('Ctrl Pts',(-1.46055812562105,1.79370633789704,0.768258557763731));
#10513=CARTESIAN_POINT('Ctrl Pts',(-1.44466308895875,1.8,0.797770130104051));
#10514=CARTESIAN_POINT('Ctrl Pts',(-1.42894191624432,1.8,0.825));
#10515=CARTESIAN_POINT('',(-1.28744468918255,1.55,1.03198167246111));
#10516=CARTESIAN_POINT('Ctrl Pts',(-1.42894191624432,1.8,0.825));
#10517=CARTESIAN_POINT('Ctrl Pts',(-1.4132207435299,1.8,0.852229869895948));
#10518=CARTESIAN_POINT('Ctrl Pts',(-1.39561049050871,1.79370633789704,0.880751161609747));
#10519=CARTESIAN_POINT('Ctrl Pts',(-1.36172049302549,1.76817777258318,0.932292094146255));
#10520=CARTESIAN_POINT('Ctrl Pts',(-1.34548213209931,1.74894552961493,0.955340251466733));
#10521=CARTESIAN_POINT('Ctrl Pts',(-1.31917543061769,1.70460745840382,0.991349264982989));
#10522=CARTESIAN_POINT('Ctrl Pts',(-1.30734972067592,1.67652816181843,1.00672880483252));
#10523=CARTESIAN_POINT('Ctrl Pts',(-1.29146042158868,1.61494799959182,1.02703269653942));
#10524=CARTESIAN_POINT('Ctrl Pts',(-1.28744468918255,1.58144291640553,1.03198167246111));
#10525=CARTESIAN_POINT('Ctrl Pts',(-1.28744468918255,1.55,1.03198167246111));
#10526=CARTESIAN_POINT('Ctrl Pts',(-1.28744468918255,1.55,1.03198167246111));
#10527=CARTESIAN_POINT('Ctrl Pts',(-1.28744468918255,1.51855708359447,1.03198167246111));
#10528=CARTESIAN_POINT('Ctrl Pts',(-1.29146042158868,1.48505200040818,1.02703269653942));
#10529=CARTESIAN_POINT('Ctrl Pts',(-1.30734972067592,1.42347183818157,1.00672880483252));
#10530=CARTESIAN_POINT('Ctrl Pts',(-1.31917543061769,1.39539254159618,0.99134926498299));
#10531=CARTESIAN_POINT('Ctrl Pts',(-1.34548213209931,1.35105447038508,0.955340251466733));
#10532=CARTESIAN_POINT('Ctrl Pts',(-1.36172049302549,1.33182222741682,0.932292094146255));
#10533=CARTESIAN_POINT('Ctrl Pts',(-1.39561049050871,1.30629366210296,0.880751161609748));
#10534=CARTESIAN_POINT('Ctrl Pts',(-1.4132207435299,1.3,0.852229869895949));
#10535=CARTESIAN_POINT('Ctrl Pts',(-1.42894191624432,1.3,0.825));
#10536=CARTESIAN_POINT('',(1.42894191624432,1.8,-0.825));
#10537=CARTESIAN_POINT('',(1.42894191624432,1.3,-0.825));
#10538=CARTESIAN_POINT('Ctrl Pts',(1.42894191624432,1.8,-0.825));
#10539=CARTESIAN_POINT('Ctrl Pts',(1.4132207435299,1.8,-0.852229869895949));
#10540=CARTESIAN_POINT('Ctrl Pts',(1.39561049050871,1.79370633789704,-0.880751161609748));
#10541=CARTESIAN_POINT('Ctrl Pts',(1.36172049302549,1.76817777258318,-0.932292094146255));
#10542=CARTESIAN_POINT('Ctrl Pts',(1.34548213209931,1.74894552961493,-0.955340251466734));
#10543=CARTESIAN_POINT('Ctrl Pts',(1.31917543061769,1.70460745840382,-0.99134926498299));
#10544=CARTESIAN_POINT('Ctrl Pts',(1.30734972067592,1.67652816181843,-1.00672880483252));
#10545=CARTESIAN_POINT('Ctrl Pts',(1.29146042158868,1.61494799959182,-1.02703269653942));
#10546=CARTESIAN_POINT('Ctrl Pts',(1.28744468918255,1.58144291640553,-1.03198167246111));
#10547=CARTESIAN_POINT('Ctrl Pts',(1.28744468918255,1.51855708359447,-1.03198167246111));
#10548=CARTESIAN_POINT('Ctrl Pts',(1.29146042158868,1.48505200040818,-1.02703269653942));
#10549=CARTESIAN_POINT('Ctrl Pts',(1.30734972067592,1.42347183818157,-1.00672880483252));
#10550=CARTESIAN_POINT('Ctrl Pts',(1.31917543061769,1.39539254159618,-0.99134926498299));
#10551=CARTESIAN_POINT('Ctrl Pts',(1.34548213209931,1.35105447038507,-0.955340251466734));
#10552=CARTESIAN_POINT('Ctrl Pts',(1.36172049302549,1.33182222741682,-0.932292094146255));
#10553=CARTESIAN_POINT('Ctrl Pts',(1.39561049050871,1.30629366210296,-0.880751161609748));
#10554=CARTESIAN_POINT('Ctrl Pts',(1.4132207435299,1.3,-0.852229869895948));
#10555=CARTESIAN_POINT('Ctrl Pts',(1.42894191624432,1.3,-0.825));
#10556=CARTESIAN_POINT('',(1.53744468918255,1.55,-0.598968970568895));
#10557=CARTESIAN_POINT('Ctrl Pts',(1.42894191624432,1.3,-0.825));
#10558=CARTESIAN_POINT('Ctrl Pts',(1.44466308895875,1.3,-0.797770130104051));
#10559=CARTESIAN_POINT('Ctrl Pts',(1.46055812562105,1.30629366210296,-0.768258557763731));
#10560=CARTESIAN_POINT('Ctrl Pts',(1.48824888379079,1.33182222741682,-0.713138492740815));
#10561=CARTESIAN_POINT('Ctrl Pts',(1.50008999307766,1.35105447038507,-0.687551581002688));
#10562=CARTESIAN_POINT('Ctrl Pts',(1.51812136280714,1.39539254159618,-0.646764802471698));
#10563=CARTESIAN_POINT('Ctrl Pts',(1.52552758004446,1.42347183818157,-0.628833667319577));
#10564=CARTESIAN_POINT('Ctrl Pts',(1.53516661651472,1.48505200040818,-0.604921184808249));
#10565=CARTESIAN_POINT('Ctrl Pts',(1.53744468918255,1.51855708359447,-0.598968970568895));
#10566=CARTESIAN_POINT('Ctrl Pts',(1.53744468918255,1.55,-0.598968970568895));
#10567=CARTESIAN_POINT('Ctrl Pts',(1.53744468918255,1.55,-0.598968970568895));
#10568=CARTESIAN_POINT('Ctrl Pts',(1.53744468918255,1.58144291640553,-0.598968970568895));
#10569=CARTESIAN_POINT('Ctrl Pts',(1.53516661651472,1.61494799959182,-0.604921184808249));
#10570=CARTESIAN_POINT('Ctrl Pts',(1.52552758004446,1.67652816181843,-0.628833667319577));
#10571=CARTESIAN_POINT('Ctrl Pts',(1.51812136280714,1.70460745840382,-0.646764802471698));
#10572=CARTESIAN_POINT('Ctrl Pts',(1.50008999307766,1.74894552961493,-0.687551581002688));
#10573=CARTESIAN_POINT('Ctrl Pts',(1.48824888379079,1.76817777258318,-0.713138492740815));
#10574=CARTESIAN_POINT('Ctrl Pts',(1.46055812562105,1.79370633789704,-0.768258557763731));
#10575=CARTESIAN_POINT('Ctrl Pts',(1.44466308895875,1.8,-0.797770130104051));
#10576=CARTESIAN_POINT('Ctrl Pts',(1.42894191624432,1.8,-0.825));
#10577=CARTESIAN_POINT('',(0.,1.3,-1.65));
#10578=CARTESIAN_POINT('',(0.,1.8,-1.65));
#10579=CARTESIAN_POINT('Ctrl Pts',(1.38777878078145E-17,1.3,-1.65));
#10580=CARTESIAN_POINT('Ctrl Pts',(0.0314423454288489,1.3,-1.65));
#10581=CARTESIAN_POINT('Ctrl Pts',(0.0649476351123396,1.30629366210296,
-1.64900971937348));
#10582=CARTESIAN_POINT('Ctrl Pts',(0.126528390765307,1.33182222741682,-1.64543058688707));
#10583=CARTESIAN_POINT('Ctrl Pts',(0.154607860978348,1.35105447038507,-1.64289183246942));
#10584=CARTESIAN_POINT('Ctrl Pts',(0.198945932189457,1.39539254159618,-1.63811406745469));
#10585=CARTESIAN_POINT('Ctrl Pts',(0.218177859368546,1.42347183818157,-1.63556247215209));
#10586=CARTESIAN_POINT('Ctrl Pts',(0.243706194926033,1.48505200040818,-1.63195388134767));
#10587=CARTESIAN_POINT('Ctrl Pts',(0.25,1.51855708359447,-1.63095064303001));
#10588=CARTESIAN_POINT('Ctrl Pts',(0.25,1.58144291640553,-1.63095064303001));
#10589=CARTESIAN_POINT('Ctrl Pts',(0.243706194926033,1.61494799959182,-1.63195388134767));
#10590=CARTESIAN_POINT('Ctrl Pts',(0.218177859368546,1.67652816181843,-1.63556247215209));
#10591=CARTESIAN_POINT('Ctrl Pts',(0.198945932189457,1.70460745840382,-1.63811406745469));
#10592=CARTESIAN_POINT('Ctrl Pts',(0.154607860978349,1.74894552961493,-1.64289183246942));
#10593=CARTESIAN_POINT('Ctrl Pts',(0.126528390765307,1.76817777258318,-1.64543058688707));
#10594=CARTESIAN_POINT('Ctrl Pts',(0.0649476351123398,1.79370633789704,
-1.64900971937348));
#10595=CARTESIAN_POINT('Ctrl Pts',(0.031442345428849,1.8,-1.65));
#10596=CARTESIAN_POINT('Ctrl Pts',(7.63278329429795E-17,1.8,-1.65));
#10597=CARTESIAN_POINT('',(-0.25,1.55,-1.63095064303001));
#10598=CARTESIAN_POINT('Ctrl Pts',(9.0205620750794E-17,1.8,-1.65));
#10599=CARTESIAN_POINT('Ctrl Pts',(-0.0314423454288488,1.8,-1.65));
#10600=CARTESIAN_POINT('Ctrl Pts',(-0.0649476351123396,1.79370633789704,
-1.64900971937348));
#10601=CARTESIAN_POINT('Ctrl Pts',(-0.126528390765307,1.76817777258318,
-1.64543058688707));
#10602=CARTESIAN_POINT('Ctrl Pts',(-0.154607860978348,1.74894552961493,
-1.64289183246942));
#10603=CARTESIAN_POINT('Ctrl Pts',(-0.198945932189456,1.70460745840382,
-1.63811406745469));
#10604=CARTESIAN_POINT('Ctrl Pts',(-0.218177859368546,1.67652816181843,
-1.63556247215209));
#10605=CARTESIAN_POINT('Ctrl Pts',(-0.243706194926033,1.61494799959182,
-1.63195388134767));
#10606=CARTESIAN_POINT('Ctrl Pts',(-0.25,1.58144291640553,-1.63095064303001));
#10607=CARTESIAN_POINT('Ctrl Pts',(-0.25,1.55,-1.63095064303001));
#10608=CARTESIAN_POINT('Ctrl Pts',(-0.25,1.55,-1.63095064303001));
#10609=CARTESIAN_POINT('Ctrl Pts',(-0.25,1.51855708359447,-1.63095064303001));
#10610=CARTESIAN_POINT('Ctrl Pts',(-0.243706194926033,1.48505200040818,
-1.63195388134767));
#10611=CARTESIAN_POINT('Ctrl Pts',(-0.218177859368546,1.42347183818157,
-1.63556247215209));
#10612=CARTESIAN_POINT('Ctrl Pts',(-0.198945932189457,1.39539254159618,
-1.63811406745469));
#10613=CARTESIAN_POINT('Ctrl Pts',(-0.154607860978349,1.35105447038507,
-1.64289183246942));
#10614=CARTESIAN_POINT('Ctrl Pts',(-0.126528390765307,1.33182222741682,
-1.64543058688707));
#10615=CARTESIAN_POINT('Ctrl Pts',(-0.0649476351123398,1.30629366210296,
-1.64900971937348));
#10616=CARTESIAN_POINT('Ctrl Pts',(-0.031442345428849,1.3,-1.65));
#10617=CARTESIAN_POINT('Ctrl Pts',(-4.85722573273506E-17,1.3,-1.65));
#10618=CARTESIAN_POINT('',(0.,1.8,1.65));
#10619=CARTESIAN_POINT('',(0.,1.3,1.65));
#10620=CARTESIAN_POINT('Ctrl Pts',(8.32667268468867E-17,1.8,1.65));
#10621=CARTESIAN_POINT('Ctrl Pts',(0.031442345428849,1.8,1.65));
#10622=CARTESIAN_POINT('Ctrl Pts',(0.0649476351123398,1.79370633789704,
1.64900971937348));
#10623=CARTESIAN_POINT('Ctrl Pts',(0.126528390765307,1.76817777258318,1.64543058688707));
#10624=CARTESIAN_POINT('Ctrl Pts',(0.154607860978349,1.74894552961493,1.64289183246942));
#10625=CARTESIAN_POINT('Ctrl Pts',(0.198945932189457,1.70460745840382,1.63811406745469));
#10626=CARTESIAN_POINT('Ctrl Pts',(0.218177859368546,1.67652816181843,1.63556247215209));
#10627=CARTESIAN_POINT('Ctrl Pts',(0.243706194926033,1.61494799959182,1.63195388134767));
#10628=CARTESIAN_POINT('Ctrl Pts',(0.25,1.58144291640553,1.63095064303001));
#10629=CARTESIAN_POINT('Ctrl Pts',(0.25,1.51855708359447,1.63095064303001));
#10630=CARTESIAN_POINT('Ctrl Pts',(0.243706194926033,1.48505200040818,1.63195388134767));
#10631=CARTESIAN_POINT('Ctrl Pts',(0.218177859368546,1.42347183818157,1.63556247215209));
#10632=CARTESIAN_POINT('Ctrl Pts',(0.198945932189457,1.39539254159618,1.63811406745469));
#10633=CARTESIAN_POINT('Ctrl Pts',(0.154607860978348,1.35105447038507,1.64289183246942));
#10634=CARTESIAN_POINT('Ctrl Pts',(0.126528390765307,1.33182222741682,1.64543058688707));
#10635=CARTESIAN_POINT('Ctrl Pts',(0.0649476351123397,1.30629366210296,
1.64900971937348));
#10636=CARTESIAN_POINT('Ctrl Pts',(0.0314423454288488,1.3,1.65));
#10637=CARTESIAN_POINT('Ctrl Pts',(-1.38777878078145E-17,1.3,1.65));
#10638=CARTESIAN_POINT('',(-0.25,1.55,1.63095064303001));
#10639=CARTESIAN_POINT('Ctrl Pts',(-5.55111512312578E-17,1.3,1.65));
#10640=CARTESIAN_POINT('Ctrl Pts',(-0.031442345428849,1.3,1.65));
#10641=CARTESIAN_POINT('Ctrl Pts',(-0.0649476351123398,1.30629366210296,
1.64900971937348));
#10642=CARTESIAN_POINT('Ctrl Pts',(-0.126528390765307,1.33182222741682,
1.64543058688707));
#10643=CARTESIAN_POINT('Ctrl Pts',(-0.154607860978349,1.35105447038507,
1.64289183246942));
#10644=CARTESIAN_POINT('Ctrl Pts',(-0.198945932189457,1.39539254159618,
1.63811406745469));
#10645=CARTESIAN_POINT('Ctrl Pts',(-0.218177859368546,1.42347183818157,
1.63556247215209));
#10646=CARTESIAN_POINT('Ctrl Pts',(-0.243706194926033,1.48505200040818,
1.63195388134767));
#10647=CARTESIAN_POINT('Ctrl Pts',(-0.25,1.51855708359447,1.63095064303001));
#10648=CARTESIAN_POINT('Ctrl Pts',(-0.25,1.55,1.63095064303001));
#10649=CARTESIAN_POINT('Ctrl Pts',(-0.25,1.55,1.63095064303001));
#10650=CARTESIAN_POINT('Ctrl Pts',(-0.25,1.58144291640553,1.63095064303001));
#10651=CARTESIAN_POINT('Ctrl Pts',(-0.243706194926033,1.61494799959182,
1.63195388134767));
#10652=CARTESIAN_POINT('Ctrl Pts',(-0.218177859368546,1.67652816181843,
1.63556247215209));
#10653=CARTESIAN_POINT('Ctrl Pts',(-0.198945932189456,1.70460745840382,
1.63811406745469));
#10654=CARTESIAN_POINT('Ctrl Pts',(-0.154607860978348,1.74894552961493,
1.64289183246942));
#10655=CARTESIAN_POINT('Ctrl Pts',(-0.126528390765307,1.76817777258318,
1.64543058688707));
#10656=CARTESIAN_POINT('Ctrl Pts',(-0.0649476351123396,1.79370633789704,
1.64900971937348));
#10657=CARTESIAN_POINT('Ctrl Pts',(-0.0314423454288488,1.8,1.65));
#10658=CARTESIAN_POINT('Ctrl Pts',(7.63278329429795E-17,1.8,1.65));
#10659=CARTESIAN_POINT('Origin',(0.,1.55,0.));
#10660=CARTESIAN_POINT('',(-0.34736109069228,1.55,0.489224153812002));
#10661=CARTESIAN_POINT('',(0.125,1.55,0.21650635094611));
#10662=CARTESIAN_POINT('Ctrl Pts',(-0.34736109069228,1.55,0.489224153812002));
#10663=CARTESIAN_POINT('Ctrl Pts',(-0.34736109069228,1.58183602855499,0.489224153812002));
#10664=CARTESIAN_POINT('Ctrl Pts',(-0.353251858758695,1.61548166177648,
0.485186294875824));
#10665=CARTESIAN_POINT('Ctrl Pts',(-0.375307371004242,1.67693412158597,
0.468334260082228));
#10666=CARTESIAN_POINT('Ctrl Pts',(-0.391292050254279,1.70478184753241,
0.455434178332924));
#10667=CARTESIAN_POINT('Ctrl Pts',(-0.425012071836758,1.74874496453875,
0.424138206994599));
#10668=CARTESIAN_POINT('Ctrl Pts',(-0.445091520936419,1.76792916820474,
0.403563860606914));
#10669=CARTESIAN_POINT('Ctrl Pts',(-0.484488022261587,1.79356669468566,
0.355304950761552));
#10670=CARTESIAN_POINT('Ctrl Pts',(-0.503716463284046,1.8,0.32753749298313));
#10671=CARTESIAN_POINT('Ctrl Pts',(-0.535514021257281,1.8,0.27246250701687));
#10672=CARTESIAN_POINT('Ctrl Pts',(-0.549947124580677,1.79356669468566,
0.241926459727038));
#10673=CARTESIAN_POINT('Ctrl Pts',(-0.572042315803119,1.76792916820474,
0.183678633836535));
#10674=CARTESIAN_POINT('Ctrl Pts',(-0.579820497891285,1.74874496453875,
0.156002147628389));
#10675=CARTESIAN_POINT('Ctrl Pts',(-0.590063593315144,1.70478184753241,
0.11115176665264));
#10676=CARTESIAN_POINT('Ctrl Pts',(-0.593243052195919,1.67693412158597,
0.0908585874761102));
#10677=CARTESIAN_POINT('Ctrl Pts',(-0.596809586309859,1.61548166177648,
0.0633319361811903));
#10678=CARTESIAN_POINT('Ctrl Pts',(-0.59736109069228,1.58183602855499,0.0562114519197831));
#10679=CARTESIAN_POINT('Ctrl Pts',(-0.59736109069228,1.51816397144501,0.0562114519197831));
#10680=CARTESIAN_POINT('Ctrl Pts',(-0.596809586309859,1.48451833822352,
0.0633319361811902));
#10681=CARTESIAN_POINT('Ctrl Pts',(-0.593243052195919,1.42306587841403,
0.0908585874761101));
#10682=CARTESIAN_POINT('Ctrl Pts',(-0.590063593315144,1.39521815246759,
0.11115176665264));
#10683=CARTESIAN_POINT('Ctrl Pts',(-0.579820497891285,1.35125503546125,
0.156002147628389));
#10684=CARTESIAN_POINT('Ctrl Pts',(-0.572042315803119,1.33207083179526,
0.183678633836535));
#10685=CARTESIAN_POINT('Ctrl Pts',(-0.549947124580676,1.30643330531434,
0.241926459727038));
#10686=CARTESIAN_POINT('Ctrl Pts',(-0.535514021257281,1.3,0.27246250701687));
#10687=CARTESIAN_POINT('Ctrl Pts',(-0.503716463284046,1.3,0.32753749298313));
#10688=CARTESIAN_POINT('Ctrl Pts',(-0.484488022261587,1.30643330531434,
0.355304950761552));
#10689=CARTESIAN_POINT('Ctrl Pts',(-0.445091520936419,1.33207083179526,
0.403563860606914));
#10690=CARTESIAN_POINT('Ctrl Pts',(-0.425012071836758,1.35125503546125,
0.424138206994599));
#10691=CARTESIAN_POINT('Ctrl Pts',(-0.391292050254279,1.39521815246759,
0.455434178332924));
#10692=CARTESIAN_POINT('Ctrl Pts',(-0.375307371004241,1.42306587841403,
0.468334260082228));
#10693=CARTESIAN_POINT('Ctrl Pts',(-0.353251858758695,1.48451833822352,
0.485186294875824));
#10694=CARTESIAN_POINT('Ctrl Pts',(-0.34736109069228,1.51816397144501,0.489224153812002));
#10695=CARTESIAN_POINT('Ctrl Pts',(-0.34736109069228,1.55,0.489224153812002));
#10696=CARTESIAN_POINT('Origin',(0.,1.55,0.));
#10697=CARTESIAN_POINT('',(0.59736109069228,1.55,-0.0562114519197831));
#10698=CARTESIAN_POINT('Ctrl Pts',(0.59736109069228,1.55,-0.0562114519197831));
#10699=CARTESIAN_POINT('Ctrl Pts',(0.59736109069228,1.51816397144501,-0.0562114519197831));
#10700=CARTESIAN_POINT('Ctrl Pts',(0.596809586309859,1.48451833822352,-0.0633319361811902));
#10701=CARTESIAN_POINT('Ctrl Pts',(0.593243052195919,1.42306587841403,-0.0908585874761101));
#10702=CARTESIAN_POINT('Ctrl Pts',(0.590063593315144,1.39521815246759,-0.11115176665264));
#10703=CARTESIAN_POINT('Ctrl Pts',(0.579820497891285,1.35125503546125,-0.156002147628389));
#10704=CARTESIAN_POINT('Ctrl Pts',(0.572042315803119,1.33207083179526,-0.183678633836535));
#10705=CARTESIAN_POINT('Ctrl Pts',(0.549947124580677,1.30643330531434,-0.241926459727038));
#10706=CARTESIAN_POINT('Ctrl Pts',(0.535514021257281,1.3,-0.27246250701687));
#10707=CARTESIAN_POINT('Ctrl Pts',(0.503716463284046,1.3,-0.32753749298313));
#10708=CARTESIAN_POINT('Ctrl Pts',(0.484488022261587,1.30643330531434,-0.355304950761552));
#10709=CARTESIAN_POINT('Ctrl Pts',(0.445091520936419,1.33207083179526,-0.403563860606914));
#10710=CARTESIAN_POINT('Ctrl Pts',(0.425012071836758,1.35125503546125,-0.424138206994599));
#10711=CARTESIAN_POINT('Ctrl Pts',(0.391292050254279,1.39521815246759,-0.455434178332924));
#10712=CARTESIAN_POINT('Ctrl Pts',(0.375307371004241,1.42306587841403,-0.468334260082228));
#10713=CARTESIAN_POINT('Ctrl Pts',(0.353251858758695,1.48451833822352,-0.485186294875824));
#10714=CARTESIAN_POINT('Ctrl Pts',(0.34736109069228,1.51816397144501,-0.489224153812002));
#10715=CARTESIAN_POINT('Ctrl Pts',(0.34736109069228,1.58183602855499,-0.489224153812002));
#10716=CARTESIAN_POINT('Ctrl Pts',(0.353251858758695,1.61548166177647,-0.485186294875824));
#10717=CARTESIAN_POINT('Ctrl Pts',(0.375307371004241,1.67693412158597,-0.468334260082228));
#10718=CARTESIAN_POINT('Ctrl Pts',(0.391292050254279,1.70478184753241,-0.455434178332924));
#10719=CARTESIAN_POINT('Ctrl Pts',(0.425012071836758,1.74874496453875,-0.424138206994599));
#10720=CARTESIAN_POINT('Ctrl Pts',(0.445091520936419,1.76792916820474,-0.403563860606914));
#10721=CARTESIAN_POINT('Ctrl Pts',(0.484488022261587,1.79356669468566,-0.355304950761552));
#10722=CARTESIAN_POINT('Ctrl Pts',(0.503716463284046,1.8,-0.32753749298313));
#10723=CARTESIAN_POINT('Ctrl Pts',(0.535514021257281,1.8,-0.27246250701687));
#10724=CARTESIAN_POINT('Ctrl Pts',(0.549947124580677,1.79356669468566,-0.241926459727038));
#10725=CARTESIAN_POINT('Ctrl Pts',(0.572042315803119,1.76792916820474,-0.183678633836535));
#10726=CARTESIAN_POINT('Ctrl Pts',(0.579820497891285,1.74874496453875,-0.156002147628389));
#10727=CARTESIAN_POINT('Ctrl Pts',(0.590063593315144,1.70478184753241,-0.111151766652641));
#10728=CARTESIAN_POINT('Ctrl Pts',(0.593243052195919,1.67693412158597,-0.0908585874761104));
#10729=CARTESIAN_POINT('Ctrl Pts',(0.596809586309859,1.61548166177648,-0.0633319361811903));
#10730=CARTESIAN_POINT('Ctrl Pts',(0.59736109069228,1.58183602855499,-0.0562114519197831));
#10731=CARTESIAN_POINT('Ctrl Pts',(0.59736109069228,1.55,-0.0562114519197831));
#10732=CARTESIAN_POINT('',(0.125,1.55,0.21650635094611));
#10733=CARTESIAN_POINT('Origin',(0.,1.55,0.));
#10734=CARTESIAN_POINT('',(-0.25,1.55,-0.545435605731786));
#10735=CARTESIAN_POINT('',(-0.25,1.55,0.));
#10736=CARTESIAN_POINT('Ctrl Pts',(-0.25,1.55,-0.545435605731786));
#10737=CARTESIAN_POINT('Ctrl Pts',(-0.25,1.58183602855499,-0.545435605731786));
#10738=CARTESIAN_POINT('Ctrl Pts',(-0.243557727551164,1.61548166177648,
-0.548518231057014));
#10739=CARTESIAN_POINT('Ctrl Pts',(-0.217935681191677,1.67693412158597,
-0.559192847558338));
#10740=CARTESIAN_POINT('Ctrl Pts',(-0.198771543060865,1.70478184753241,
-0.566585944985565));
#10741=CARTESIAN_POINT('Ctrl Pts',(-0.154808426054527,1.74874496453875,
-0.580140354622989));
#10742=CARTESIAN_POINT('Ctrl Pts',(-0.1269507948667,1.76792916820474,-0.587242494443449));
#10743=CARTESIAN_POINT('Ctrl Pts',(-0.0654591023190899,1.79356669468566,
-0.597231410488591));
#10744=CARTESIAN_POINT('Ctrl Pts',(-0.0317975579732349,1.8,-0.6));
#10745=CARTESIAN_POINT('Ctrl Pts',(0.0317975579732349,1.8,-0.6));
#10746=CARTESIAN_POINT('Ctrl Pts',(0.0654591023190898,1.79356669468566,
-0.597231410488591));
#10747=CARTESIAN_POINT('Ctrl Pts',(0.1269507948667,1.76792916820474,-0.587242494443449));
#10748=CARTESIAN_POINT('Ctrl Pts',(0.154808426054527,1.74874496453875,-0.580140354622989));
#10749=CARTESIAN_POINT('Ctrl Pts',(0.198771543060865,1.70478184753241,-0.566585944985565));
#10750=CARTESIAN_POINT('Ctrl Pts',(0.217935681191677,1.67693412158597,-0.559192847558338));
#10751=CARTESIAN_POINT('Ctrl Pts',(0.243557727551164,1.61548166177648,-0.548518231057014));
#10752=CARTESIAN_POINT('Ctrl Pts',(0.25,1.58183602855499,-0.545435605731786));
#10753=CARTESIAN_POINT('Ctrl Pts',(0.25,1.51816397144501,-0.545435605731786));
#10754=CARTESIAN_POINT('Ctrl Pts',(0.243557727551164,1.48451833822352,-0.548518231057014));
#10755=CARTESIAN_POINT('Ctrl Pts',(0.217935681191677,1.42306587841403,-0.559192847558338));
#10756=CARTESIAN_POINT('Ctrl Pts',(0.198771543060865,1.39521815246759,-0.566585944985565));
#10757=CARTESIAN_POINT('Ctrl Pts',(0.154808426054527,1.35125503546125,-0.580140354622989));
#10758=CARTESIAN_POINT('Ctrl Pts',(0.1269507948667,1.33207083179526,-0.587242494443449));
#10759=CARTESIAN_POINT('Ctrl Pts',(0.0654591023190899,1.30643330531434,
-0.597231410488591));
#10760=CARTESIAN_POINT('Ctrl Pts',(0.0317975579732349,1.3,-0.6));
#10761=CARTESIAN_POINT('Ctrl Pts',(-0.0317975579732349,1.3,-0.6));
#10762=CARTESIAN_POINT('Ctrl Pts',(-0.0654591023190899,1.30643330531434,
-0.597231410488591));
#10763=CARTESIAN_POINT('Ctrl Pts',(-0.1269507948667,1.33207083179526,-0.587242494443449));
#10764=CARTESIAN_POINT('Ctrl Pts',(-0.154808426054527,1.35125503546125,
-0.580140354622989));
#10765=CARTESIAN_POINT('Ctrl Pts',(-0.198771543060865,1.39521815246759,
-0.566585944985565));
#10766=CARTESIAN_POINT('Ctrl Pts',(-0.217935681191677,1.42306587841403,
-0.559192847558338));
#10767=CARTESIAN_POINT('Ctrl Pts',(-0.243557727551164,1.48451833822352,
-0.548518231057014));
#10768=CARTESIAN_POINT('Ctrl Pts',(-0.25,1.51816397144501,-0.545435605731786));
#10769=CARTESIAN_POINT('Ctrl Pts',(-0.25,1.55,-0.545435605731786));
#10770=CARTESIAN_POINT('Origin',(0.,1.55,0.));
#10771=CARTESIAN_POINT('',(-0.25,1.55,0.545435605731786));
#10772=CARTESIAN_POINT('Ctrl Pts',(-0.25,1.55,0.545435605731786));
#10773=CARTESIAN_POINT('Ctrl Pts',(-0.25,1.51816397144501,0.545435605731786));
#10774=CARTESIAN_POINT('Ctrl Pts',(-0.243557727551164,1.48451833822352,
0.548518231057014));
#10775=CARTESIAN_POINT('Ctrl Pts',(-0.217935681191677,1.42306587841403,
0.559192847558338));
#10776=CARTESIAN_POINT('Ctrl Pts',(-0.198771543060865,1.39521815246759,
0.566585944985565));
#10777=CARTESIAN_POINT('Ctrl Pts',(-0.154808426054527,1.35125503546125,
0.580140354622989));
#10778=CARTESIAN_POINT('Ctrl Pts',(-0.1269507948667,1.33207083179526,0.587242494443449));
#10779=CARTESIAN_POINT('Ctrl Pts',(-0.0654591023190899,1.30643330531434,
0.597231410488591));
#10780=CARTESIAN_POINT('Ctrl Pts',(-0.0317975579732349,1.3,0.6));
#10781=CARTESIAN_POINT('Ctrl Pts',(0.0317975579732349,1.3,0.6));
#10782=CARTESIAN_POINT('Ctrl Pts',(0.0654591023190899,1.30643330531434,
0.597231410488591));
#10783=CARTESIAN_POINT('Ctrl Pts',(0.1269507948667,1.33207083179526,0.587242494443449));
#10784=CARTESIAN_POINT('Ctrl Pts',(0.154808426054527,1.35125503546125,0.580140354622989));
#10785=CARTESIAN_POINT('Ctrl Pts',(0.198771543060865,1.39521815246759,0.566585944985565));
#10786=CARTESIAN_POINT('Ctrl Pts',(0.217935681191677,1.42306587841403,0.559192847558338));
#10787=CARTESIAN_POINT('Ctrl Pts',(0.243557727551164,1.48451833822352,0.548518231057014));
#10788=CARTESIAN_POINT('Ctrl Pts',(0.25,1.51816397144501,0.545435605731786));
#10789=CARTESIAN_POINT('Ctrl Pts',(0.25,1.58183602855499,0.545435605731786));
#10790=CARTESIAN_POINT('Ctrl Pts',(0.243557727551164,1.61548166177648,0.548518231057014));
#10791=CARTESIAN_POINT('Ctrl Pts',(0.217935681191677,1.67693412158597,0.559192847558338));
#10792=CARTESIAN_POINT('Ctrl Pts',(0.198771543060865,1.70478184753241,0.566585944985565));
#10793=CARTESIAN_POINT('Ctrl Pts',(0.154808426054527,1.74874496453875,0.580140354622989));
#10794=CARTESIAN_POINT('Ctrl Pts',(0.1269507948667,1.76792916820474,0.587242494443449));
#10795=CARTESIAN_POINT('Ctrl Pts',(0.0654591023190898,1.79356669468566,
0.597231410488591));
#10796=CARTESIAN_POINT('Ctrl Pts',(0.0317975579732349,1.8,0.6));
#10797=CARTESIAN_POINT('Ctrl Pts',(-0.0317975579732349,1.8,0.6));
#10798=CARTESIAN_POINT('Ctrl Pts',(-0.0654591023190898,1.79356669468566,
0.597231410488591));
#10799=CARTESIAN_POINT('Ctrl Pts',(-0.1269507948667,1.76792916820474,0.587242494443449));
#10800=CARTESIAN_POINT('Ctrl Pts',(-0.154808426054527,1.74874496453875,
0.580140354622989));
#10801=CARTESIAN_POINT('Ctrl Pts',(-0.198771543060865,1.70478184753241,
0.566585944985565));
#10802=CARTESIAN_POINT('Ctrl Pts',(-0.217935681191677,1.67693412158597,
0.559192847558339));
#10803=CARTESIAN_POINT('Ctrl Pts',(-0.243557727551164,1.61548166177648,
0.548518231057014));
#10804=CARTESIAN_POINT('Ctrl Pts',(-0.25,1.58183602855499,0.545435605731786));
#10805=CARTESIAN_POINT('Ctrl Pts',(-0.25,1.55,0.545435605731786));
#10806=CARTESIAN_POINT('',(-0.25,1.55,0.));
#10807=CARTESIAN_POINT('Origin',(1.65,2.25,0.));
#10808=CARTESIAN_POINT('',(-0.6,2.25,-7.34788079488412E-17));
#10809=CARTESIAN_POINT('Origin',(0.,2.25,0.));
#10810=CARTESIAN_POINT('Origin',(1.75,0.85,0.));
#10811=CARTESIAN_POINT('',(-1.75,0.85,-2.14313189850787E-16));
#10812=CARTESIAN_POINT('Origin',(0.,0.85,0.));
#10813=CARTESIAN_POINT('Origin',(0.,0.,0.));
#10814=CARTESIAN_POINT('',(-1.75,-0.85,-2.14313189850787E-16));
#10815=CARTESIAN_POINT('Origin',(0.,-0.85,0.));
#10816=CARTESIAN_POINT('',(-1.75,0.,-2.14313189850787E-16));
#10817=CARTESIAN_POINT('Origin',(0.6,-0.85,0.));
#10818=CARTESIAN_POINT('',(-0.6,-0.85,-7.34788079488412E-17));
#10819=CARTESIAN_POINT('Origin',(0.,-0.85,0.));
#10820=CARTESIAN_POINT('Origin',(0.,0.7,0.));
#10821=CARTESIAN_POINT('',(-0.6,0.7,-7.34788079488412E-17));
#10822=CARTESIAN_POINT('',(0.,0.,0.));
#10823=CARTESIAN_POINT('',(0.,0.,0.));
#10824=CARTESIAN_POINT('',(0.,0.,0.));
#10825=CARTESIAN_POINT('Origin',(0.6,0.8,0.));
#10826=CARTESIAN_POINT('',(-0.6,0.8,-7.34788079488412E-17));
#10827=CARTESIAN_POINT('Origin',(0.,0.8,0.));
#10828=CARTESIAN_POINT('Origin',(0.,0.775,0.));
#10829=CARTESIAN_POINT('',(-0.65,0.75,-7.9602041944578E-17));
#10830=CARTESIAN_POINT('Origin',(0.,0.75,0.));
#10831=CARTESIAN_POINT('',(-0.625,0.775,-7.65404249467096E-17));
#10832=CARTESIAN_POINT('Origin',(0.,0.39,0.));
#10833=CARTESIAN_POINT('',(-0.65,0.0299999999999998,-7.9602041944578E-17));
#10834=CARTESIAN_POINT('Origin',(0.,0.0299999999999998,0.));
#10835=CARTESIAN_POINT('',(-0.65,0.39,-7.9602041944578E-17));
#10836=CARTESIAN_POINT('Origin',(0.,0.0150000000000001,0.));
#10837=CARTESIAN_POINT('',(-0.62,5.89805981832114E-17,-7.59281015471359E-17));
#10838=CARTESIAN_POINT('Origin',(0.,0.,0.));
#10839=CARTESIAN_POINT('',(-0.635,0.0150000000000001,-7.77650717458569E-17));
#10840=CARTESIAN_POINT('Origin',(0.42,0.,0.));
#10841=CARTESIAN_POINT('',(-0.42,-3.46944695195361E-18,-5.14351655641888E-17));
#10842=CARTESIAN_POINT('Origin',(0.,0.,0.));
#10843=CARTESIAN_POINT('Origin',(0.,-0.02,0.));
#10844=CARTESIAN_POINT('',(-0.3933,-0.0534000000000001,4.81653586104654E-17));
#10845=CARTESIAN_POINT('Origin',(0.,-0.0534000000000001,0.));
#10846=CARTESIAN_POINT('',(-0.41,-0.02,-5.02105187650415E-17));
#10847=CARTESIAN_POINT('Origin',(0.,-1.48,0.));
#10848=CARTESIAN_POINT('',(-0.3933,-2.9267,4.81653586104654E-17));
#10849=CARTESIAN_POINT('Origin',(0.,-2.9267,0.));
#10850=CARTESIAN_POINT('',(-0.3933,-1.48,-4.81653586104654E-17));
#10851=CARTESIAN_POINT('Origin',(0.,-2.96,0.));
#10852=CARTESIAN_POINT('',(-0.32,-3.,-3.91886975727153E-17));
#10853=CARTESIAN_POINT('Origin',(0.,-3.,0.));
#10854=CARTESIAN_POINT('',(-0.36,-2.96,-4.40872847693047E-17));
#10855=CARTESIAN_POINT('Origin',(0.,-3.,0.));
#10856=CARTESIAN_POINT('Origin',(0.173205080756888,-0.8,-0.3));
#10857=CARTESIAN_POINT('',(0.346410161513775,-0.8,0.));
#10858=CARTESIAN_POINT('',(0.173205080756888,-0.8,-0.3));
#10859=CARTESIAN_POINT('',(0.346410161513775,-0.8,0.));
#10860=CARTESIAN_POINT('',(0.173205080756888,-1.28,-0.3));
#10861=CARTESIAN_POINT('',(0.173205080756888,-0.8,-0.3));
#10862=CARTESIAN_POINT('',(0.346410161513775,-1.28,0.));
#10863=CARTESIAN_POINT('',(0.346410161513775,-1.28,0.));
#10864=CARTESIAN_POINT('',(0.346410161513775,-0.8,0.));
#10865=CARTESIAN_POINT('Origin',(-0.173205080756888,-0.8,-0.3));
#10866=CARTESIAN_POINT('',(-0.173205080756888,-0.8,-0.3));
#10867=CARTESIAN_POINT('',(0.173205080756888,-0.8,-0.3));
#10868=CARTESIAN_POINT('',(-0.173205080756888,-1.28,-0.3));
#10869=CARTESIAN_POINT('',(-0.173205080756888,-0.8,-0.3));
#10870=CARTESIAN_POINT('',(0.173205080756888,-1.28,-0.3));
#10871=CARTESIAN_POINT('Origin',(-0.346410161513775,-0.8,-5.55111512312578E-17));
#10872=CARTESIAN_POINT('',(-0.346410161513775,-0.8,-4.24230095489963E-17));
#10873=CARTESIAN_POINT('',(-0.173205080756888,-0.8,-0.3));
#10874=CARTESIAN_POINT('',(-0.346410161513775,-1.28,-5.55111512312578E-17));
#10875=CARTESIAN_POINT('',(-0.346410161513775,-0.8,-4.24230095489963E-17));
#10876=CARTESIAN_POINT('',(-0.173205080756888,-1.28,-0.3));
#10877=CARTESIAN_POINT('Origin',(-0.173205080756888,-0.8,0.3));
#10878=CARTESIAN_POINT('',(-0.173205080756888,-0.8,0.3));
#10879=CARTESIAN_POINT('',(-0.346410161513775,-0.8,-4.24230095489963E-17));
#10880=CARTESIAN_POINT('',(-0.173205080756888,-1.28,0.3));
#10881=CARTESIAN_POINT('',(-0.173205080756888,-0.8,0.3));
#10882=CARTESIAN_POINT('',(-0.346410161513775,-1.28,-4.24230095489963E-17));
#10883=CARTESIAN_POINT('Origin',(0.173205080756888,-0.8,0.3));
#10884=CARTESIAN_POINT('',(0.173205080756888,-0.8,0.3));
#10885=CARTESIAN_POINT('',(-0.173205080756888,-0.8,0.3));
#10886=CARTESIAN_POINT('',(0.173205080756888,-1.28,0.3));
#10887=CARTESIAN_POINT('',(0.173205080756888,-0.8,0.3));
#10888=CARTESIAN_POINT('',(-0.173205080756888,-1.28,0.3));
#10889=CARTESIAN_POINT('Origin',(0.346410161513775,-0.8,0.));
#10890=CARTESIAN_POINT('',(0.173205080756888,-0.8,0.3));
#10891=CARTESIAN_POINT('',(0.173205080756888,-1.28,0.3));
#10892=CARTESIAN_POINT('Origin',(0.,-0.8,-5.55111512312578E-17));
#10893=CARTESIAN_POINT('Origin',(0.,-1.28,-5.55111512312578E-17));
#10894=CARTESIAN_POINT('',(0.,0.,0.));
#10895=CARTESIAN_POINT('Origin',(0.,0.,0.));
#10896=CARTESIAN_POINT('',(-0.42,0.16,5.14351655641888E-17));
#10897=CARTESIAN_POINT('Origin',(0.,0.16,0.));
#10898=CARTESIAN_POINT('',(-0.42,0.,5.14351655641888E-17));
#10899=CARTESIAN_POINT('',(-0.42,0.,5.14351655641888E-17));
#10900=CARTESIAN_POINT('Origin',(0.,0.,0.));
#10901=CARTESIAN_POINT('Origin',(0.,0.,0.));
#10902=CARTESIAN_POINT('',(-0.8,0.16,9.79717439317883E-17));
#10903=CARTESIAN_POINT('Origin',(0.,0.16,0.));
#10904=CARTESIAN_POINT('',(-0.8,0.,9.79717439317883E-17));
#10905=CARTESIAN_POINT('',(-0.8,0.,9.79717439317883E-17));
#10906=CARTESIAN_POINT('Origin',(0.,0.,0.));
#10907=CARTESIAN_POINT('Origin',(0.,0.16,0.));
#10908=CARTESIAN_POINT('Origin',(0.,0.,0.));
#10909=CARTESIAN_POINT('',(0.,0.,0.));
#10910=CARTESIAN_POINT('Origin',(0.,0.067277284513851,0.));
#10911=CARTESIAN_POINT('',(-0.375277674973257,0.0768195421087395,0.65));
#10912=CARTESIAN_POINT('',(0.375277674973257,0.0768195421087395,0.65));
#10913=CARTESIAN_POINT('Ctrl Pts',(-0.375277674973257,0.0768195421087395,
0.65));
#10914=CARTESIAN_POINT('Ctrl Pts',(1.66533453693773E-13,-0.0315137912242439,
0.65));
#10915=CARTESIAN_POINT('Ctrl Pts',(0.375277674973257,0.0768195421087394,
0.65));
#10916=CARTESIAN_POINT('',(-0.750555349946514,0.0768195421087394,-9.19165206894919E-17));
#10917=CARTESIAN_POINT('Ctrl Pts',(-0.750555349946514,0.0768195421087394,
-9.19165206894919E-17));
#10918=CARTESIAN_POINT('Ctrl Pts',(-0.562916512459802,-0.0315137912242434,
0.325000000000144));
#10919=CARTESIAN_POINT('Ctrl Pts',(-0.375277674973257,0.0768195421087395,
0.65));
#10920=CARTESIAN_POINT('',(-0.6175,-2.77555756156289E-17,-7.5621939847349E-17));
#10921=CARTESIAN_POINT('',(-0.734027674973257,0.067277284513851,-8.98924642641573E-17));
#10922=CARTESIAN_POINT('Origin',(0.,0.,0.));
#10923=CARTESIAN_POINT('',(-0.375277674973257,0.0768195421087395,-0.65));
#10924=CARTESIAN_POINT('Ctrl Pts',(-0.375277674973257,0.0768195421087395,
-0.65));
#10925=CARTESIAN_POINT('Ctrl Pts',(-0.562916512459968,-0.0315137912242437,
-0.324999999999856));
#10926=CARTESIAN_POINT('Ctrl Pts',(-0.750555349946514,0.0768195421087395,
-9.19165206894919E-17));
#10927=CARTESIAN_POINT('',(0.375277674973257,0.0768195421087395,-0.65));
#10928=CARTESIAN_POINT('Ctrl Pts',(0.375277674973257,0.0768195421087395,
-0.65));
#10929=CARTESIAN_POINT('Ctrl Pts',(-1.66144875635155E-13,-0.0315137912242437,
-0.65));
#10930=CARTESIAN_POINT('Ctrl Pts',(-0.375277674973257,0.0768195421087395,
-0.65));
#10931=CARTESIAN_POINT('',(0.750555349946514,0.0768195421087394,0.));
#10932=CARTESIAN_POINT('Ctrl Pts',(0.750555349946514,0.0768195421087394,
0.));
#10933=CARTESIAN_POINT('Ctrl Pts',(0.562916512459802,-0.0315137912242436,
-0.325000000000144));
#10934=CARTESIAN_POINT('Ctrl Pts',(0.375277674973257,0.0768195421087395,
-0.65));
#10935=CARTESIAN_POINT('Ctrl Pts',(0.375277674973257,0.0768195421087394,
0.65));
#10936=CARTESIAN_POINT('Ctrl Pts',(0.562916512459968,-0.0315137912242439,
0.324999999999856));
#10937=CARTESIAN_POINT('Ctrl Pts',(0.750555349946514,0.0768195421087394,
0.));
#10938=CARTESIAN_POINT('Origin',(0.,0.612722715486149,0.));
#10939=CARTESIAN_POINT('',(-0.6175,0.68,-7.5621939847349E-17));
#10940=CARTESIAN_POINT('Origin',(0.,0.68,0.));
#10941=CARTESIAN_POINT('',(-0.750555349946514,0.603180457891261,-9.19165206894919E-17));
#10942=CARTESIAN_POINT('',(-0.734027674973257,0.612722715486149,-8.98924642641573E-17));
#10943=CARTESIAN_POINT('',(-0.375277674973257,0.603180457891261,0.65));
#10944=CARTESIAN_POINT('Ctrl Pts',(-0.375277674973257,0.603180457891261,
0.65));
#10945=CARTESIAN_POINT('Ctrl Pts',(-0.562916512459968,0.711513791224243,
0.324999999999856));
#10946=CARTESIAN_POINT('Ctrl Pts',(-0.750555349946514,0.603180457891261,
-9.19165206894919E-17));
#10947=CARTESIAN_POINT('',(0.375277674973257,0.603180457891261,0.65));
#10948=CARTESIAN_POINT('Ctrl Pts',(0.375277674973257,0.603180457891261,
0.65));
#10949=CARTESIAN_POINT('Ctrl Pts',(-1.66755498298699E-13,0.711513791224244,
0.65));
#10950=CARTESIAN_POINT('Ctrl Pts',(-0.375277674973257,0.603180457891261,
0.65));
#10951=CARTESIAN_POINT('',(0.750555349946514,0.603180457891261,0.));
#10952=CARTESIAN_POINT('Ctrl Pts',(0.750555349946514,0.603180457891261,
0.));
#10953=CARTESIAN_POINT('Ctrl Pts',(0.562916512459802,0.711513791224244,
0.325000000000144));
#10954=CARTESIAN_POINT('Ctrl Pts',(0.375277674973257,0.603180457891261,
0.65));
#10955=CARTESIAN_POINT('',(0.375277674973257,0.603180457891261,-0.65));
#10956=CARTESIAN_POINT('Ctrl Pts',(0.375277674973257,0.603180457891261,
-0.65));
#10957=CARTESIAN_POINT('Ctrl Pts',(0.562916512459969,0.711513791224244,
-0.324999999999856));
#10958=CARTESIAN_POINT('Ctrl Pts',(0.750555349946514,0.603180457891261,
0.));
#10959=CARTESIAN_POINT('',(-0.375277674973257,0.603180457891261,-0.65));
#10960=CARTESIAN_POINT('Ctrl Pts',(-0.375277674973257,0.603180457891261,
-0.65));
#10961=CARTESIAN_POINT('Ctrl Pts',(1.66422431391311E-13,0.711513791224244,
-0.65));
#10962=CARTESIAN_POINT('Ctrl Pts',(0.375277674973257,0.603180457891261,
-0.65));
#10963=CARTESIAN_POINT('Ctrl Pts',(-0.750555349946514,0.603180457891261,
-9.19165206894919E-17));
#10964=CARTESIAN_POINT('Ctrl Pts',(-0.562916512459802,0.711513791224244,
-0.325000000000144));
#10965=CARTESIAN_POINT('Ctrl Pts',(-0.375277674973257,0.603180457891261,
-0.65));
#10966=CARTESIAN_POINT('Origin',(0.375277674973257,0.,-0.65));
#10967=CARTESIAN_POINT('',(-0.375277674973257,0.,-0.65));
#10968=CARTESIAN_POINT('',(0.375277674973257,0.,-0.65));
#10969=CARTESIAN_POINT('Origin',(-0.375277674973257,0.,-0.65));
#10970=CARTESIAN_POINT('',(-0.750555349946514,0.,-9.19165206894919E-17));
#10971=CARTESIAN_POINT('Origin',(-0.750555349946514,0.,-9.19165206894919E-17));
#10972=CARTESIAN_POINT('',(-0.375277674973257,0.,0.65));
#10973=CARTESIAN_POINT('Origin',(0.,0.,0.));
#10974=CARTESIAN_POINT('',(-0.338975,0.68,4.15124648740974E-17));
#10975=CARTESIAN_POINT('Origin',(0.,0.68,0.));
#10976=CARTESIAN_POINT('',(-0.338975,0.,4.15124648740974E-17));
#10977=CARTESIAN_POINT('',(-0.338975,0.,4.15124648740974E-17));
#10978=CARTESIAN_POINT('Origin',(0.,0.,0.));
#10979=CARTESIAN_POINT('Origin',(-0.375277674973257,0.,0.65));
#10980=CARTESIAN_POINT('',(0.375277674973257,0.,0.65));
#10981=CARTESIAN_POINT('Origin',(0.750555349946514,0.,0.));
#10982=CARTESIAN_POINT('',(0.750555349946514,0.,0.));
#10983=CARTESIAN_POINT('Origin',(0.375277674973257,0.,0.65));
#10984=CARTESIAN_POINT('Origin',(0.,0.68,-1.11022302462516E-16));
#10985=CARTESIAN_POINT('Origin',(0.,0.,-1.11022302462516E-16));
#10986=CARTESIAN_POINT('',(0.,0.,0.));
#10987=CARTESIAN_POINT('',(0.,0.,0.));
#10988=CARTESIAN_POINT('',(0.,0.,0.));
#10989=CARTESIAN_POINT('',(0.,0.,0.));
#10990=CARTESIAN_POINT('',(0.,0.,0.));
#10991=CARTESIAN_POINT('',(0.,0.,0.));
#10992=CARTESIAN_POINT('',(0.,0.,0.));
#10993=CARTESIAN_POINT('',(0.,0.,0.));
#10994=CARTESIAN_POINT('',(0.,0.,0.));
#10995=CARTESIAN_POINT('',(0.,0.,0.));
#10996=CARTESIAN_POINT('',(0.,0.,0.));
#10997=CARTESIAN_POINT('',(0.,0.,0.));
#10998=CARTESIAN_POINT('',(0.,0.,0.));
#10999=CARTESIAN_POINT('',(0.,0.,0.));
#11000=CARTESIAN_POINT('',(0.,0.,0.));
#11001=CARTESIAN_POINT('',(-10.,-3.,1.));
#11002=CARTESIAN_POINT('',(-7.,-3.,1.42));
#11003=CARTESIAN_POINT('',(-7.,-3.,3.2));
#11004=CARTESIAN_POINT('',(7.,-3.,1.42));
#11005=CARTESIAN_POINT('',(7.,-3.,3.2));
#11006=CARTESIAN_POINT('',(-10.,5.,1.));
#11007=CARTESIAN_POINT('',(-7.,5.,1.42));
#11008=CARTESIAN_POINT('',(-7.,5.,3.2));
#11009=CARTESIAN_POINT('',(7.,5.,1.42));
#11010=CARTESIAN_POINT('',(7.,5.,3.2));
#11011=CARTESIAN_POINT('',(-10.,13.,1.));
#11012=CARTESIAN_POINT('',(-7.,13.,1.42));
#11013=CARTESIAN_POINT('',(-7.,13.,3.2));
#11014=CARTESIAN_POINT('',(7.,13.,1.42));
#11015=CARTESIAN_POINT('',(7.,13.,3.2));
#11016=CARTESIAN_POINT('',(-10.,21.,1.));
#11017=CARTESIAN_POINT('',(-7.,21.,1.42));
#11018=CARTESIAN_POINT('',(-7.,21.,3.2));
#11019=CARTESIAN_POINT('',(7.,21.,1.42));
#11020=CARTESIAN_POINT('',(7.,21.,3.2));
#11021=CARTESIAN_POINT('',(-5.,-2.5,4.2));
#11022=CARTESIAN_POINT('',(5.,-2.5,4.2));
#11023=CARTESIAN_POINT('',(0.,0.,10.));
#11024=CARTESIAN_POINT('',(-3.2,0.5,6.8));
#11025=CARTESIAN_POINT('',(-3.2,0.66,6.8));
#11026=CARTESIAN_POINT('',(-3.2,-1.46,6.8));
#11027=CARTESIAN_POINT('',(-3.2,-2.14,6.8));
#11028=CARTESIAN_POINT('',(-3.2,0.5,13.2));
#11029=CARTESIAN_POINT('',(-3.2,0.66,13.2));
#11030=CARTESIAN_POINT('',(-3.2,-1.46,13.2));
#11031=CARTESIAN_POINT('',(-3.2,-2.14,13.2));
#11032=CARTESIAN_POINT('',(3.2,0.5,6.8));
#11033=CARTESIAN_POINT('',(3.2,0.66,6.8));
#11034=CARTESIAN_POINT('',(3.2,-1.46,6.8));
#11035=CARTESIAN_POINT('',(3.2,-2.14,6.8));
#11036=CARTESIAN_POINT('',(3.2,0.5,13.2));
#11037=CARTESIAN_POINT('',(3.2,0.66,13.2));
#11038=CARTESIAN_POINT('',(3.2,-1.46,13.2));
#11039=CARTESIAN_POINT('',(3.2,-2.14,13.2));
#11040=CARTESIAN_POINT('',(-5.,15.5,4.2));
#11041=CARTESIAN_POINT('',(5.,15.5,4.2));
#11042=CARTESIAN_POINT('',(0.,18.,10.));
#11043=CARTESIAN_POINT('',(-3.2,18.5,6.8));
#11044=CARTESIAN_POINT('',(-3.2,18.66,6.8));
#11045=CARTESIAN_POINT('',(-3.2,16.54,6.8));
#11046=CARTESIAN_POINT('',(-3.2,15.86,6.8));
#11047=CARTESIAN_POINT('',(-3.2,18.5,13.2));
#11048=CARTESIAN_POINT('',(-3.2,18.66,13.2));
#11049=CARTESIAN_POINT('',(-3.2,16.54,13.2));
#11050=CARTESIAN_POINT('',(-3.2,15.86,13.2));
#11051=CARTESIAN_POINT('',(3.2,18.5,6.8));
#11052=CARTESIAN_POINT('',(3.2,18.66,6.8));
#11053=CARTESIAN_POINT('',(3.2,16.54,6.8));
#11054=CARTESIAN_POINT('',(3.2,15.86,6.8));
#11055=CARTESIAN_POINT('',(3.2,18.5,13.2));
#11056=CARTESIAN_POINT('',(3.2,18.66,13.2));
#11057=CARTESIAN_POINT('',(3.2,16.54,13.2));
#11058=CARTESIAN_POINT('',(3.2,15.86,13.2));
#11059=CARTESIAN_POINT('',(0.,0.,0.));
#11060=CARTESIAN_POINT('',(0.,0.,0.));
#11061=CARTESIAN_POINT('Origin',(-0.2,7.775,9.3));
#11062=CARTESIAN_POINT('',(-0.2,9.225,9.43431457505076));
#11063=CARTESIAN_POINT('',(-0.2,7.775,9.43431457505076));
#11064=CARTESIAN_POINT('',(-0.2,-3.5,9.43431457505076));
#11065=CARTESIAN_POINT('',(-0.2,9.225,9.65));
#11066=CARTESIAN_POINT('',(-0.2,9.225,9.65));
#11067=CARTESIAN_POINT('',(-0.2,7.775,9.65));
#11068=CARTESIAN_POINT('',(-0.2,7.775,9.65));
#11069=CARTESIAN_POINT('',(-0.2,7.775,9.65));
#11070=CARTESIAN_POINT('Origin',(0.,7.775,9.475));
#11071=CARTESIAN_POINT('',(0.2,7.775,9.43431457505076));
#11072=CARTESIAN_POINT('Origin',(0.,7.775,10.));
#11073=CARTESIAN_POINT('',(0.2,7.775,9.65));
#11074=CARTESIAN_POINT('',(0.2,7.775,9.65));
#11075=CARTESIAN_POINT('',(0.2,7.775,9.3));
#11076=CARTESIAN_POINT('Origin',(0.2,7.775,9.65));
#11077=CARTESIAN_POINT('',(0.2,9.225,9.43431457505076));
#11078=CARTESIAN_POINT('',(0.2,-3.5,9.43431457505076));
#11079=CARTESIAN_POINT('',(0.2,9.225,9.65));
#11080=CARTESIAN_POINT('',(0.2,7.775,9.65));
#11081=CARTESIAN_POINT('',(0.2,9.225,9.3));
#11082=CARTESIAN_POINT('Origin',(-0.2,7.775,9.65));
#11083=CARTESIAN_POINT('',(0.2,9.225,9.65));
#11084=CARTESIAN_POINT('Origin',(0.,9.225,9.475));
#11085=CARTESIAN_POINT('Origin',(0.,9.225,10.));
#11086=CARTESIAN_POINT('Origin',(0.,-1.665,10.));
#11087=CARTESIAN_POINT('',(-1.,-1.665,10.));
#11088=CARTESIAN_POINT('Origin',(0.,-1.665,10.));
#11089=CARTESIAN_POINT('',(-0.6,-1.665,10.));
#11090=CARTESIAN_POINT('Origin',(0.,-1.665,10.));
#11091=CARTESIAN_POINT('Origin',(0.,-2.,10.));
#11092=CARTESIAN_POINT('',(-1.,-2.,10.));
#11093=CARTESIAN_POINT('Origin',(0.,-2.,10.));
#11094=CARTESIAN_POINT('',(-0.6,-2.,10.));
#11095=CARTESIAN_POINT('Origin',(0.,-2.,10.));
#11096=CARTESIAN_POINT('Origin',(0.,-2.,10.));
#11097=CARTESIAN_POINT('',(-1.,-2.,10.));
#11098=CARTESIAN_POINT('Origin',(0.,-3.5,10.));
#11099=CARTESIAN_POINT('',(-0.6,-3.5,10.));
#11100=CARTESIAN_POINT('',(-0.6,-3.5,10.));
#11101=CARTESIAN_POINT('Origin',(0.,-3.5,10.));
#11102=CARTESIAN_POINT('Origin',(0.,-3.5,10.));
#11103=CARTESIAN_POINT('',(-0.6,24.5,10.));
#11104=CARTESIAN_POINT('Origin',(0.,24.5,10.));
#11105=CARTESIAN_POINT('',(-0.6,-3.5,10.));
#11106=CARTESIAN_POINT('Origin',(0.,24.5,10.));
#11107=CARTESIAN_POINT('Origin',(0.,-3.5,10.));
#11108=CARTESIAN_POINT('',(0.,0.,0.));
#11109=CARTESIAN_POINT('Origin',(0.,-1.665,10.));
#11110=CARTESIAN_POINT('',(-0.605,-0.85,10.));
#11111=CARTESIAN_POINT('Origin',(0.,-0.85,10.));
#11112=CARTESIAN_POINT('',(-0.605,-1.665,10.));
#11113=CARTESIAN_POINT('',(-0.605,-1.665,10.));
#11114=CARTESIAN_POINT('Origin',(0.,-1.665,10.));
#11115=CARTESIAN_POINT('Origin',(0.,-1.665,10.));
#11116=CARTESIAN_POINT('',(-1.,-0.85,10.));
#11117=CARTESIAN_POINT('Origin',(0.,-0.85,10.));
#11118=CARTESIAN_POINT('',(-1.,-1.665,10.));
#11119=CARTESIAN_POINT('',(-1.,-1.665,10.));
#11120=CARTESIAN_POINT('Origin',(0.,-1.665,10.));
#11121=CARTESIAN_POINT('Origin',(0.,-0.85,10.));
#11122=CARTESIAN_POINT('Origin',(0.,-1.665,10.));
#11123=CARTESIAN_POINT('',(0.,0.,0.));
#11124=CARTESIAN_POINT('Origin',(0.,20.45,10.));
#11125=CARTESIAN_POINT('',(-0.605,21.,10.));
#11126=CARTESIAN_POINT('Origin',(0.,21.,10.));
#11127=CARTESIAN_POINT('',(-0.605,20.45,10.));
#11128=CARTESIAN_POINT('',(-0.605,20.45,10.));
#11129=CARTESIAN_POINT('Origin',(0.,20.45,10.));
#11130=CARTESIAN_POINT('Origin',(0.,20.45,10.));
#11131=CARTESIAN_POINT('',(-1.,21.,10.));
#11132=CARTESIAN_POINT('Origin',(0.,21.,10.));
#11133=CARTESIAN_POINT('',(-1.,20.45,10.));
#11134=CARTESIAN_POINT('',(-1.,20.45,10.));
#11135=CARTESIAN_POINT('Origin',(0.,20.45,10.));
#11136=CARTESIAN_POINT('Origin',(0.,21.,10.));
#11137=CARTESIAN_POINT('Origin',(0.,20.45,10.));
#11138=CARTESIAN_POINT('',(0.,0.,0.));
#11139=CARTESIAN_POINT('Origin',(0.,20.9,10.));
#11140=CARTESIAN_POINT('',(-0.54,21.,10.));
#11141=CARTESIAN_POINT('Origin',(0.,21.,10.));
#11142=CARTESIAN_POINT('',(-0.54,21.8,10.));
#11143=CARTESIAN_POINT('',(-0.54,20.9,10.));
#11144=CARTESIAN_POINT('Origin',(0.,21.8,10.));
#11145=CARTESIAN_POINT('Origin',(1.09696551146029,21.,10.));
#11146=CARTESIAN_POINT('',(0.548482755730145,21.,9.05));
#11147=CARTESIAN_POINT('',(1.09696551146029,21.,10.));
#11148=CARTESIAN_POINT('',(0.548482755730145,21.,9.05));
#11149=CARTESIAN_POINT('',(0.548482755730145,21.8,9.05));
#11150=CARTESIAN_POINT('',(0.548482755730145,21.,9.05));
#11151=CARTESIAN_POINT('',(1.09696551146029,21.8,10.));
#11152=CARTESIAN_POINT('',(0.548482755730145,21.8,9.05));
#11153=CARTESIAN_POINT('',(1.09696551146029,21.,10.));
#11154=CARTESIAN_POINT('Origin',(0.548482755730145,21.,10.95));
#11155=CARTESIAN_POINT('',(0.548482755730145,21.,10.95));
#11156=CARTESIAN_POINT('',(1.09696551146029,21.,10.));
#11157=CARTESIAN_POINT('',(0.548482755730145,21.8,10.95));
#11158=CARTESIAN_POINT('',(1.09696551146029,21.8,10.));
#11159=CARTESIAN_POINT('',(0.548482755730145,21.,10.95));
#11160=CARTESIAN_POINT('Origin',(-0.548482755730144,21.,10.95));
#11161=CARTESIAN_POINT('',(-0.548482755730144,21.,10.95));
#11162=CARTESIAN_POINT('',(0.548482755730145,21.,10.95));
#11163=CARTESIAN_POINT('',(-0.548482755730144,21.8,10.95));
#11164=CARTESIAN_POINT('',(0.548482755730145,21.8,10.95));
#11165=CARTESIAN_POINT('',(-0.548482755730144,21.,10.95));
#11166=CARTESIAN_POINT('Origin',(-1.09696551146029,21.,10.));
#11167=CARTESIAN_POINT('',(-1.09696551146029,21.,10.));
#11168=CARTESIAN_POINT('',(-0.548482755730144,21.,10.95));
#11169=CARTESIAN_POINT('',(-1.09696551146029,21.8,10.));
#11170=CARTESIAN_POINT('',(-0.548482755730144,21.8,10.95));
#11171=CARTESIAN_POINT('',(-1.09696551146029,21.,10.));
#11172=CARTESIAN_POINT('Origin',(-0.548482755730145,21.,9.05));
#11173=CARTESIAN_POINT('',(-0.548482755730145,21.,9.05));
#11174=CARTESIAN_POINT('',(-1.09696551146029,21.,10.));
#11175=CARTESIAN_POINT('',(-0.548482755730145,21.8,9.05));
#11176=CARTESIAN_POINT('',(-1.09696551146029,21.8,10.));
#11177=CARTESIAN_POINT('',(-0.548482755730145,21.,9.05));
#11178=CARTESIAN_POINT('Origin',(0.548482755730145,21.,9.05));
#11179=CARTESIAN_POINT('',(-0.548482755730145,21.,9.05));
#11180=CARTESIAN_POINT('',(-0.548482755730145,21.8,9.05));
#11181=CARTESIAN_POINT('Origin',(0.,21.8,10.));
#11182=CARTESIAN_POINT('Origin',(0.,21.,10.));
#11183=CARTESIAN_POINT('',(0.,0.,0.));
#11184=CARTESIAN_POINT('Origin',(0.,21.7,10.));
#11185=CARTESIAN_POINT('',(-0.54,21.8,10.));
#11186=CARTESIAN_POINT('Origin',(0.,21.8,10.));
#11187=CARTESIAN_POINT('',(-0.54,22.6,10.));
#11188=CARTESIAN_POINT('',(-0.54,21.7,10.));
#11189=CARTESIAN_POINT('Origin',(0.,22.6,10.));
#11190=CARTESIAN_POINT('Origin',(1.09696551146029,21.8,10.));
#11191=CARTESIAN_POINT('',(0.548482755730145,21.8,9.05));
#11192=CARTESIAN_POINT('',(1.09696551146029,21.8,10.));
#11193=CARTESIAN_POINT('',(0.548482755730145,21.8,9.05));
#11194=CARTESIAN_POINT('',(0.548482755730145,22.6,9.05));
#11195=CARTESIAN_POINT('',(0.548482755730145,21.8,9.05));
#11196=CARTESIAN_POINT('',(1.09696551146029,22.6,10.));
#11197=CARTESIAN_POINT('',(0.548482755730145,22.6,9.05));
#11198=CARTESIAN_POINT('',(1.09696551146029,21.8,10.));
#11199=CARTESIAN_POINT('Origin',(0.548482755730145,21.8,10.95));
#11200=CARTESIAN_POINT('',(0.548482755730145,21.8,10.95));
#11201=CARTESIAN_POINT('',(1.09696551146029,21.8,10.));
#11202=CARTESIAN_POINT('',(0.548482755730145,22.6,10.95));
#11203=CARTESIAN_POINT('',(1.09696551146029,22.6,10.));
#11204=CARTESIAN_POINT('',(0.548482755730145,21.8,10.95));
#11205=CARTESIAN_POINT('Origin',(-0.548482755730144,21.8,10.95));
#11206=CARTESIAN_POINT('',(-0.548482755730144,21.8,10.95));
#11207=CARTESIAN_POINT('',(0.548482755730145,21.8,10.95));
#11208=CARTESIAN_POINT('',(-0.548482755730144,22.6,10.95));
#11209=CARTESIAN_POINT('',(0.548482755730145,22.6,10.95));
#11210=CARTESIAN_POINT('',(-0.548482755730144,21.8,10.95));
#11211=CARTESIAN_POINT('Origin',(-1.09696551146029,21.8,10.));
#11212=CARTESIAN_POINT('',(-1.09696551146029,21.8,10.));
#11213=CARTESIAN_POINT('',(-0.548482755730144,21.8,10.95));
#11214=CARTESIAN_POINT('',(-1.09696551146029,22.6,10.));
#11215=CARTESIAN_POINT('',(-0.548482755730144,22.6,10.95));
#11216=CARTESIAN_POINT('',(-1.09696551146029,21.8,10.));
#11217=CARTESIAN_POINT('Origin',(-0.548482755730145,21.8,9.05));
#11218=CARTESIAN_POINT('',(-0.548482755730145,21.8,9.05));
#11219=CARTESIAN_POINT('',(-1.09696551146029,21.8,10.));
#11220=CARTESIAN_POINT('',(-0.548482755730145,22.6,9.05));
#11221=CARTESIAN_POINT('',(-1.09696551146029,22.6,10.));
#11222=CARTESIAN_POINT('',(-0.548482755730145,21.8,9.05));
#11223=CARTESIAN_POINT('Origin',(0.548482755730145,21.8,9.05));
#11224=CARTESIAN_POINT('',(-0.548482755730145,21.8,9.05));
#11225=CARTESIAN_POINT('',(-0.548482755730145,22.6,9.05));
#11226=CARTESIAN_POINT('Origin',(0.,22.6,10.));
#11227=CARTESIAN_POINT('Origin',(0.,21.8,10.));
#11228=CARTESIAN_POINT('',(0.,0.,0.));
#11229=CARTESIAN_POINT('Origin',(0.,7.5,10.59));
#11230=CARTESIAN_POINT('',(0.109087121146348,7.32055641555073,10.59));
#11231=CARTESIAN_POINT('',(0.109087121146348,7.67944358444927,10.59));
#11232=CARTESIAN_POINT('',(0.109087121146348,7.,10.59));
#11233=CARTESIAN_POINT('Origin',(0.,7.5,10.59));
#11234=CARTESIAN_POINT('Origin',(0.,7.5,10.59));
#11235=CARTESIAN_POINT('',(-0.109087121146348,7.32055641555073,10.59));
#11236=CARTESIAN_POINT('Ctrl Pts',(-0.109087121146348,7.32055641555073,
10.59));
#11237=CARTESIAN_POINT('Ctrl Pts',(-0.100058962329427,7.31506802844783,
10.5916692472112));
#11238=CARTESIAN_POINT('Ctrl Pts',(-0.0905297208284634,7.31021510111871,
10.5932143633855));
#11239=CARTESIAN_POINT('Ctrl Pts',(-0.0548356965671431,7.29536302924048,
10.598057680137));
#11240=CARTESIAN_POINT('Ctrl Pts',(-0.026606099485122,7.29,10.6));
#11241=CARTESIAN_POINT('Ctrl Pts',(0.0266060994851219,7.29,10.6));
#11242=CARTESIAN_POINT('Ctrl Pts',(0.054835696567143,7.29536302924048,10.598057680137));
#11243=CARTESIAN_POINT('Ctrl Pts',(0.0905297208284634,7.31021510111871,
10.5932143633855));
#11244=CARTESIAN_POINT('Ctrl Pts',(0.100058962329428,7.31506802844783,10.5916692472112));
#11245=CARTESIAN_POINT('Ctrl Pts',(0.109087121146348,7.32055641555073,10.59));
#11246=CARTESIAN_POINT('',(-0.21,7.5,10.59));
#11247=CARTESIAN_POINT('Origin',(0.,7.5,10.59));
#11248=CARTESIAN_POINT('',(-0.21,7.5,11.4852272553384));
#11249=CARTESIAN_POINT('',(-0.21,7.5,10.59));
#11250=CARTESIAN_POINT('',(0.21,7.5,11.4852272553384));
#11251=CARTESIAN_POINT('Ctrl Pts',(0.21,7.5,11.4852272553384));
#11252=CARTESIAN_POINT('Ctrl Pts',(0.21,7.47359447307555,11.4852272553384));
#11253=CARTESIAN_POINT('Ctrl Pts',(0.204715737269596,7.44545292590929,11.4860041595441));
#11254=CARTESIAN_POINT('Ctrl Pts',(0.183273763036332,7.39372373109487,11.4888007328232));
#11255=CARTESIAN_POINT('Ctrl Pts',(0.167117923970394,7.37013307587204,11.4907789715758));
#11256=CARTESIAN_POINT('Ctrl Pts',(0.129867169887369,7.33288232178902,11.4944848114133));
#11257=CARTESIAN_POINT('Ctrl Pts',(0.106276408305765,7.31672628999865,11.4964545565713));
#11258=CARTESIAN_POINT('Ctrl Pts',(0.0545468514059003,7.29528417517378,
11.4992316551565));
#11259=CARTESIAN_POINT('Ctrl Pts',(0.0264051785092814,7.29,11.5));
#11260=CARTESIAN_POINT('Ctrl Pts',(-0.0264051785092814,7.29,11.5));
#11261=CARTESIAN_POINT('Ctrl Pts',(-0.0545468514059002,7.29528417517378,
11.4992316551565));
#11262=CARTESIAN_POINT('Ctrl Pts',(-0.106276408305765,7.31672628999865,
11.4964545565713));
#11263=CARTESIAN_POINT('Ctrl Pts',(-0.129867169887369,7.33288232178902,
11.4944848114133));
#11264=CARTESIAN_POINT('Ctrl Pts',(-0.167117923970394,7.37013307587204,
11.4907789715758));
#11265=CARTESIAN_POINT('Ctrl Pts',(-0.183273763036332,7.39372373109487,
11.4888007328232));
#11266=CARTESIAN_POINT('Ctrl Pts',(-0.204715737269596,7.44545292590929,
11.4860041595441));
#11267=CARTESIAN_POINT('Ctrl Pts',(-0.21,7.47359447307555,11.4852272553384));
#11268=CARTESIAN_POINT('Ctrl Pts',(-0.21,7.5,11.4852272553384));
#11269=CARTESIAN_POINT('Ctrl Pts',(-0.21,7.5,11.4852272553384));
#11270=CARTESIAN_POINT('Ctrl Pts',(-0.21,7.52640552692445,11.4852272553384));
#11271=CARTESIAN_POINT('Ctrl Pts',(-0.204715737269596,7.55454707409071,
11.4860041595441));
#11272=CARTESIAN_POINT('Ctrl Pts',(-0.183273763036332,7.60627626890513,
11.4888007328232));
#11273=CARTESIAN_POINT('Ctrl Pts',(-0.167117923970394,7.62986692412796,
11.4907789715758));
#11274=CARTESIAN_POINT('Ctrl Pts',(-0.129867169887369,7.66711767821098,
11.4944848114133));
#11275=CARTESIAN_POINT('Ctrl Pts',(-0.106276408305765,7.68327371000135,
11.4964545565713));
#11276=CARTESIAN_POINT('Ctrl Pts',(-0.0545468514059003,7.70471582482622,
11.4992316551565));
#11277=CARTESIAN_POINT('Ctrl Pts',(-0.0264051785092814,7.71,11.5));
#11278=CARTESIAN_POINT('Ctrl Pts',(0.0264051785092813,7.71,11.5));
#11279=CARTESIAN_POINT('Ctrl Pts',(0.0545468514059002,7.70471582482622,
11.4992316551565));
#11280=CARTESIAN_POINT('Ctrl Pts',(0.106276408305765,7.68327371000135,11.4964545565713));
#11281=CARTESIAN_POINT('Ctrl Pts',(0.129867169887369,7.66711767821098,11.4944848114133));
#11282=CARTESIAN_POINT('Ctrl Pts',(0.167117923970394,7.62986692412796,11.4907789715758));
#11283=CARTESIAN_POINT('Ctrl Pts',(0.183273763036332,7.60627626890513,11.4888007328232));
#11284=CARTESIAN_POINT('Ctrl Pts',(0.204715737269596,7.55454707409071,11.4860041595441));
#11285=CARTESIAN_POINT('Ctrl Pts',(0.21,7.52640552692445,11.4852272553384));
#11286=CARTESIAN_POINT('Ctrl Pts',(0.21,7.5,11.4852272553384));
#11287=CARTESIAN_POINT('',(-0.109087121146348,7.67944358444927,10.59));
#11288=CARTESIAN_POINT('Origin',(0.,7.5,10.59));
#11289=CARTESIAN_POINT('Ctrl Pts',(0.109087121146348,7.67944358444927,10.59));
#11290=CARTESIAN_POINT('Ctrl Pts',(0.100058962329428,7.68493197155217,10.5916692472112));
#11291=CARTESIAN_POINT('Ctrl Pts',(0.0905297208284629,7.68978489888129,
10.5932143633855));
#11292=CARTESIAN_POINT('Ctrl Pts',(0.054835696567143,7.70463697075952,10.598057680137));
#11293=CARTESIAN_POINT('Ctrl Pts',(0.026606099485122,7.71,10.6));
#11294=CARTESIAN_POINT('Ctrl Pts',(-0.0266060994851219,7.71,10.6));
#11295=CARTESIAN_POINT('Ctrl Pts',(-0.054835696567143,7.70463697075952,
10.598057680137));
#11296=CARTESIAN_POINT('Ctrl Pts',(-0.0905297208284633,7.68978489888129,
10.5932143633855));
#11297=CARTESIAN_POINT('Ctrl Pts',(-0.100058962329427,7.68493197155217,
10.5916692472112));
#11298=CARTESIAN_POINT('Ctrl Pts',(-0.109087121146348,7.67944358444927,
10.59));
#11299=CARTESIAN_POINT('Origin',(0.,7.5,10.59));
#11300=CARTESIAN_POINT('',(-0.109087121146348,7.,10.59));
#11301=CARTESIAN_POINT('Origin',(-0.2,6.9,9.22));
#11302=CARTESIAN_POINT('',(-0.2,7.,9.22));
#11303=CARTESIAN_POINT('',(-0.2,7.,9.43431457505076));
#11304=CARTESIAN_POINT('',(-0.2,7.,9.61));
#11305=CARTESIAN_POINT('',(-0.2,10.,9.22));
#11306=CARTESIAN_POINT('',(-0.2,6.9,9.22));
#11307=CARTESIAN_POINT('',(-0.2,10.,9.43431457505076));
#11308=CARTESIAN_POINT('',(-0.2,10.,9.61));
#11309=CARTESIAN_POINT('',(-0.2,7.,9.43431457505076));
#11310=CARTESIAN_POINT('Origin',(0.2,6.9,9.22));
#11311=CARTESIAN_POINT('',(0.2,7.,9.22));
#11312=CARTESIAN_POINT('',(0.1,7.,9.22));
#11313=CARTESIAN_POINT('',(0.2,10.,9.22));
#11314=CARTESIAN_POINT('',(0.2,6.9,9.22));
#11315=CARTESIAN_POINT('',(0.1,10.,9.22));
#11316=CARTESIAN_POINT('Origin',(0.2,6.9,10.));
#11317=CARTESIAN_POINT('',(0.2,7.,9.43431457505076));
#11318=CARTESIAN_POINT('',(0.2,7.,10.));
#11319=CARTESIAN_POINT('',(0.2,10.,9.43431457505076));
#11320=CARTESIAN_POINT('',(0.2,7.,9.43431457505076));
#11321=CARTESIAN_POINT('',(0.2,10.,10.));
#11322=CARTESIAN_POINT('Origin',(0.,10.,10.));
#11323=CARTESIAN_POINT('',(-1.5,10.,10.));
#11324=CARTESIAN_POINT('Origin',(0.,10.,10.));
#11325=CARTESIAN_POINT('Origin',(0.,10.,10.));
#11326=CARTESIAN_POINT('Origin',(0.,7.,10.));
#11327=CARTESIAN_POINT('Origin',(0.,7.,10.));
#11328=CARTESIAN_POINT('Origin',(-2.2,7.9,10.));
#11329=CARTESIAN_POINT('',(-2.475,8.,10.));
#11330=CARTESIAN_POINT('Origin',(-2.2,8.,10.));
#11331=CARTESIAN_POINT('',(-2.475,9.,10.));
#11332=CARTESIAN_POINT('',(-2.475,7.9,10.));
#11333=CARTESIAN_POINT('Origin',(-2.2,9.,10.));
#11334=CARTESIAN_POINT('Origin',(1.34711147906209E-16,7.9,12.2));
#11335=CARTESIAN_POINT('',(-0.275,8.,12.2));
#11336=CARTESIAN_POINT('Origin',(1.34711147906209E-16,8.,12.2));
#11337=CARTESIAN_POINT('',(-0.275,9.,12.2));
#11338=CARTESIAN_POINT('',(-0.275,7.9,12.2));
#11339=CARTESIAN_POINT('Origin',(1.34711147906209E-16,9.,12.2));
#11340=CARTESIAN_POINT('Origin',(2.2,7.9,10.));
#11341=CARTESIAN_POINT('',(1.925,8.,10.));
#11342=CARTESIAN_POINT('Origin',(2.2,8.,10.));
#11343=CARTESIAN_POINT('',(1.925,9.,10.));
#11344=CARTESIAN_POINT('',(1.925,7.9,10.));
#11345=CARTESIAN_POINT('Origin',(2.2,9.,10.));
#11346=CARTESIAN_POINT('Origin',(-4.04133443718627E-16,7.9,7.8));
#11347=CARTESIAN_POINT('',(-0.275,8.,7.8));
#11348=CARTESIAN_POINT('Origin',(-4.04133443718627E-16,8.,7.8));
#11349=CARTESIAN_POINT('',(-0.275,9.,7.8));
#11350=CARTESIAN_POINT('',(-0.275,7.9,7.8));
#11351=CARTESIAN_POINT('Origin',(-4.04133443718627E-16,9.,7.8));
#11352=CARTESIAN_POINT('Origin',(0.,9.,10.));
#11353=CARTESIAN_POINT('',(-3.,9.,10.));
#11354=CARTESIAN_POINT('Origin',(0.,9.,10.));
#11355=CARTESIAN_POINT('',(-1.5,9.,10.));
#11356=CARTESIAN_POINT('Origin',(0.,9.,10.));
#11357=CARTESIAN_POINT('Origin',(0.,8.,10.));
#11358=CARTESIAN_POINT('',(-3.,8.,10.));
#11359=CARTESIAN_POINT('Origin',(0.,8.,10.));
#11360=CARTESIAN_POINT('',(-1.5,8.,10.));
#11361=CARTESIAN_POINT('Origin',(0.,8.,10.));
#11362=CARTESIAN_POINT('Origin',(0.,8.,10.));
#11363=CARTESIAN_POINT('',(-3.,8.,10.));
#11364=CARTESIAN_POINT('Origin',(0.,7.,10.));
#11365=CARTESIAN_POINT('',(-1.5,7.,10.));
#11366=CARTESIAN_POINT('',(-1.5,7.,10.));
#11367=CARTESIAN_POINT('Origin',(0.,7.,10.));
#11368=CARTESIAN_POINT('Origin',(0.,7.,10.));
#11369=CARTESIAN_POINT('',(-1.5,7.,10.));
#11370=CARTESIAN_POINT('Origin',(0.,7.,10.));
#11371=CARTESIAN_POINT('',(0.,0.,0.));
#11372=CARTESIAN_POINT('Origin',(0.7,0.,0.25));
#11373=CARTESIAN_POINT('',(0.7,0.16,0.4));
#11374=CARTESIAN_POINT('',(0.7,0.2,0.36));
#11375=CARTESIAN_POINT('',(0.7,0.1675,0.3925));
#11376=CARTESIAN_POINT('',(0.7,-0.16,0.4));
#11377=CARTESIAN_POINT('',(0.7,0.,0.4));
#11378=CARTESIAN_POINT('',(0.7,-0.2,0.36));
#11379=CARTESIAN_POINT('',(0.7,-0.1675,0.3925));
#11380=CARTESIAN_POINT('',(0.7,-0.2,0.04));
#11381=CARTESIAN_POINT('',(0.7,-0.2,0.125));
#11382=CARTESIAN_POINT('',(0.7,-0.16,0.));
#11383=CARTESIAN_POINT('',(0.7,-0.1925,0.0325));
#11384=CARTESIAN_POINT('',(0.7,0.16,0.));
#11385=CARTESIAN_POINT('',(0.7,0.,0.));
#11386=CARTESIAN_POINT('',(0.7,0.2,0.04));
#11387=CARTESIAN_POINT('',(0.7,0.1925,0.0325));
#11388=CARTESIAN_POINT('',(0.7,0.2,0.125));
#11389=CARTESIAN_POINT('Origin',(-0.4,-0.18,0.02));
#11390=CARTESIAN_POINT('',(-0.7,-0.2,0.04));
#11391=CARTESIAN_POINT('',(-0.4,-0.2,0.04));
#11392=CARTESIAN_POINT('',(-0.7,-0.16,0.));
#11393=CARTESIAN_POINT('',(-0.7,-0.1925,0.0325));
#11394=CARTESIAN_POINT('',(-0.4,-0.16,0.));
#11395=CARTESIAN_POINT('Origin',(-0.8,-0.2,0.));
#11396=CARTESIAN_POINT('',(-0.7,-0.2,0.36));
#11397=CARTESIAN_POINT('',(-0.4,-0.2,0.36));
#11398=CARTESIAN_POINT('',(-0.7,-0.2,0.125));
#11399=CARTESIAN_POINT('Origin',(-0.4,-0.18,0.38));
#11400=CARTESIAN_POINT('',(-0.7,-0.16,0.4));
#11401=CARTESIAN_POINT('',(-0.4,-0.16,0.4));
#11402=CARTESIAN_POINT('',(-0.7,-0.1675,0.3925));
#11403=CARTESIAN_POINT('Origin',(0.,0.,0.4));
#11404=CARTESIAN_POINT('',(-0.7,0.16,0.4));
#11405=CARTESIAN_POINT('',(0.4,0.16,0.4));
#11406=CARTESIAN_POINT('',(-0.7,0.,0.4));
#11407=CARTESIAN_POINT('Origin',(-0.7,0.,0.25));
#11408=CARTESIAN_POINT('',(-0.7,0.2,0.36));
#11409=CARTESIAN_POINT('',(-0.7,0.1675,0.3925));
#11410=CARTESIAN_POINT('',(-0.7,0.2,0.04));
#11411=CARTESIAN_POINT('',(-0.7,0.2,0.125));
#11412=CARTESIAN_POINT('',(-0.7,0.16,0.));
#11413=CARTESIAN_POINT('',(-0.7,0.1925,0.0325));
#11414=CARTESIAN_POINT('',(-0.7,0.,0.));
#11415=CARTESIAN_POINT('Origin',(0.4,0.18,0.38));
#11416=CARTESIAN_POINT('',(0.4,0.2,0.36));
#11417=CARTESIAN_POINT('Origin',(0.8,0.2,0.));
#11418=CARTESIAN_POINT('',(0.4,0.2,0.04));
#11419=CARTESIAN_POINT('Origin',(0.4,0.18,0.02));
#11420=CARTESIAN_POINT('',(0.4,0.16,0.));
#11421=CARTESIAN_POINT('Origin',(0.,0.,0.));
#11422=CARTESIAN_POINT('',(0.,0.,0.));
#11423=CARTESIAN_POINT('Origin',(0.0721687836487032,0.,-0.125));
#11424=CARTESIAN_POINT('',(0.0721687836487032,0.,-0.125));
#11425=CARTESIAN_POINT('',(0.144337567297406,0.,0.));
#11426=CARTESIAN_POINT('',(0.117710979560879,0.,-0.0461186027918559));
#11427=CARTESIAN_POINT('',(0.0721687836487032,-0.25,-0.125));
#11428=CARTESIAN_POINT('',(0.0721687836487032,0.,-0.125));
#11429=CARTESIAN_POINT('',(0.144337567297406,-0.25,0.));
#11430=CARTESIAN_POINT('',(0.144337567297406,-0.25,0.));
#11431=CARTESIAN_POINT('',(0.144337567297406,0.,0.));
#11432=CARTESIAN_POINT('Origin',(-0.0721687836487032,0.,-0.125));
#11433=CARTESIAN_POINT('',(-0.0721687836487032,0.,-0.125));
#11434=CARTESIAN_POINT('',(0.0739156081756484,0.,-0.125));
#11435=CARTESIAN_POINT('',(-0.0721687836487032,-0.25,-0.125));
#11436=CARTESIAN_POINT('',(-0.0721687836487032,0.,-0.125));
#11437=CARTESIAN_POINT('',(0.0721687836487032,-0.25,-0.125));
#11438=CARTESIAN_POINT('Origin',(-0.144337567297406,0.,-4.16333634234434E-17));
#11439=CARTESIAN_POINT('',(-0.144337567297406,0.,-1.76762539787485E-17));
#11440=CARTESIAN_POINT('',(-0.0987953713852306,0.,-0.0788813972081442));
#11441=CARTESIAN_POINT('',(-0.144337567297406,-0.25,-2.77555756156289E-17));
#11442=CARTESIAN_POINT('',(-0.144337567297406,0.,-1.76762539787485E-17));
#11443=CARTESIAN_POINT('',(-0.0721687836487032,-0.25,-0.125));
#11444=CARTESIAN_POINT('Origin',(-0.0721687836487033,0.,0.125));
#11445=CARTESIAN_POINT('',(-0.0721687836487033,0.,0.125));
#11446=CARTESIAN_POINT('',(-0.0627109795608791,0.,0.141381397208144));
#11447=CARTESIAN_POINT('',(-0.0721687836487033,-0.25,0.125));
#11448=CARTESIAN_POINT('',(-0.0721687836487033,0.,0.125));
#11449=CARTESIAN_POINT('',(-0.144337567297406,-0.25,-1.76762539787485E-17));
#11450=CARTESIAN_POINT('Origin',(0.0721687836487032,0.,0.125));
#11451=CARTESIAN_POINT('',(0.0721687836487032,0.,0.125));
#11452=CARTESIAN_POINT('',(0.146084391824352,0.,0.125));
#11453=CARTESIAN_POINT('',(0.0721687836487032,-0.25,0.125));
#11454=CARTESIAN_POINT('',(0.0721687836487032,0.,0.125));
#11455=CARTESIAN_POINT('',(-0.0721687836487033,-0.25,0.125));
#11456=CARTESIAN_POINT('Origin',(0.144337567297406,0.,0.));
#11457=CARTESIAN_POINT('',(0.153795371385231,0.,-0.0163813972081441));
#11458=CARTESIAN_POINT('',(0.0721687836487032,-0.25,0.125));
#11459=CARTESIAN_POINT('Origin',(0.,-0.25,0.));
#11460=CARTESIAN_POINT('Origin',(0.22,0.,0.));
#11461=CARTESIAN_POINT('',(-0.22,-8.67361737988404E-18,-2.69422295812418E-17));
#11462=CARTESIAN_POINT('Origin',(0.,0.,0.));
#11463=CARTESIAN_POINT('Origin',(0.,-0.015,0.));
#11464=CARTESIAN_POINT('',(-0.24505,-0.02505,-3.00099698131059E-17));
#11465=CARTESIAN_POINT('Origin',(0.,-0.02505,0.));
#11466=CARTESIAN_POINT('',(-0.235,-0.015,-2.87791997799628E-17));
#11467=CARTESIAN_POINT('Origin',(0.,-0.3775,0.));
#11468=CARTESIAN_POINT('',(-0.24505,-0.72995,3.00099698131059E-17));
#11469=CARTESIAN_POINT('Origin',(0.,-0.72995,0.));
#11470=CARTESIAN_POINT('',(-0.24505,-0.3775,-3.00099698131059E-17));
#11471=CARTESIAN_POINT('Origin',(0.,-0.7625,0.));
#11472=CARTESIAN_POINT('',(-0.175,-0.8,-2.14313189850787E-17));
#11473=CARTESIAN_POINT('Origin',(0.,-0.8,0.));
#11474=CARTESIAN_POINT('',(-0.2125,-0.7625,-2.60237444818813E-17));
#11475=CARTESIAN_POINT('Origin',(0.,-0.8,0.));
#11476=CARTESIAN_POINT('',(0.,0.,0.));
#11477=CARTESIAN_POINT('',(0.,0.,0.));
#11478=CARTESIAN_POINT('',(0.,0.,0.));
#11479=CARTESIAN_POINT('',(0.,0.,0.));
#11480=CARTESIAN_POINT('',(0.,0.,0.));
#11481=CARTESIAN_POINT('',(0.,0.,0.));
#11482=CARTESIAN_POINT('',(0.,8.5,9.65));
#11483=CARTESIAN_POINT('',(0.,7.5,11.4));
#11484=CARTESIAN_POINT('',(0.,0.,0.));
#11485=CARTESIAN_POINT('',(0.,0.,0.));
#11486=UNCERTAINTY_MEASURE_WITH_UNIT(LENGTH_MEASURE(0.001),#11560,
'DISTANCE_ACCURACY_VALUE',
'Maximum model space distance between geometric entities at asserted c
onnectivities');
#11487=UNCERTAINTY_MEASURE_WITH_UNIT(LENGTH_MEASURE(0.001),#11560,
'DISTANCE_ACCURACY_VALUE',
'Maximum model space distance between geometric entities at asserted c
onnectivities');
#11488=UNCERTAINTY_MEASURE_WITH_UNIT(LENGTH_MEASURE(0.001),#11560,
'DISTANCE_ACCURACY_VALUE',
'Maximum model space distance between geometric entities at asserted c
onnectivities');
#11489=UNCERTAINTY_MEASURE_WITH_UNIT(LENGTH_MEASURE(0.001),#11560,
'DISTANCE_ACCURACY_VALUE',
'Maximum model space distance between geometric entities at asserted c
onnectivities');
#11490=UNCERTAINTY_MEASURE_WITH_UNIT(LENGTH_MEASURE(0.001),#11560,
'DISTANCE_ACCURACY_VALUE',
'Maximum model space distance between geometric entities at asserted c
onnectivities');
#11491=UNCERTAINTY_MEASURE_WITH_UNIT(LENGTH_MEASURE(0.001),#11560,
'DISTANCE_ACCURACY_VALUE',
'Maximum model space distance between geometric entities at asserted c
onnectivities');
#11492=UNCERTAINTY_MEASURE_WITH_UNIT(LENGTH_MEASURE(0.001),#11560,
'DISTANCE_ACCURACY_VALUE',
'Maximum model space distance between geometric entities at asserted c
onnectivities');
#11493=UNCERTAINTY_MEASURE_WITH_UNIT(LENGTH_MEASURE(0.001),#11560,
'DISTANCE_ACCURACY_VALUE',
'Maximum model space distance between geometric entities at asserted c
onnectivities');
#11494=UNCERTAINTY_MEASURE_WITH_UNIT(LENGTH_MEASURE(0.001),#11560,
'DISTANCE_ACCURACY_VALUE',
'Maximum model space distance between geometric entities at asserted c
onnectivities');
#11495=UNCERTAINTY_MEASURE_WITH_UNIT(LENGTH_MEASURE(0.001),#11560,
'DISTANCE_ACCURACY_VALUE',
'Maximum model space distance between geometric entities at asserted c
onnectivities');
#11496=UNCERTAINTY_MEASURE_WITH_UNIT(LENGTH_MEASURE(0.001),#11560,
'DISTANCE_ACCURACY_VALUE',
'Maximum model space distance between geometric entities at asserted c
onnectivities');
#11497=UNCERTAINTY_MEASURE_WITH_UNIT(LENGTH_MEASURE(0.001),#11560,
'DISTANCE_ACCURACY_VALUE',
'Maximum model space distance between geometric entities at asserted c
onnectivities');
#11498=UNCERTAINTY_MEASURE_WITH_UNIT(LENGTH_MEASURE(0.001),#11560,
'DISTANCE_ACCURACY_VALUE',
'Maximum model space distance between geometric entities at asserted c
onnectivities');
#11499=UNCERTAINTY_MEASURE_WITH_UNIT(LENGTH_MEASURE(0.001),#11560,
'DISTANCE_ACCURACY_VALUE',
'Maximum model space distance between geometric entities at asserted c
onnectivities');
#11500=UNCERTAINTY_MEASURE_WITH_UNIT(LENGTH_MEASURE(0.001),#11560,
'DISTANCE_ACCURACY_VALUE',
'Maximum model space distance between geometric entities at asserted c
onnectivities');
#11501=UNCERTAINTY_MEASURE_WITH_UNIT(LENGTH_MEASURE(0.001),#11560,
'DISTANCE_ACCURACY_VALUE',
'Maximum model space distance between geometric entities at asserted c
onnectivities');
#11502=UNCERTAINTY_MEASURE_WITH_UNIT(LENGTH_MEASURE(0.001),#11560,
'DISTANCE_ACCURACY_VALUE',
'Maximum model space distance between geometric entities at asserted c
onnectivities');
#11503=UNCERTAINTY_MEASURE_WITH_UNIT(LENGTH_MEASURE(0.001),#11560,
'DISTANCE_ACCURACY_VALUE',
'Maximum model space distance between geometric entities at asserted c
onnectivities');
#11504=UNCERTAINTY_MEASURE_WITH_UNIT(LENGTH_MEASURE(0.001),#11560,
'DISTANCE_ACCURACY_VALUE',
'Maximum model space distance between geometric entities at asserted c
onnectivities');
#11505=UNCERTAINTY_MEASURE_WITH_UNIT(LENGTH_MEASURE(0.001),#11560,
'DISTANCE_ACCURACY_VALUE',
'Maximum model space distance between geometric entities at asserted c
onnectivities');
#11506=UNCERTAINTY_MEASURE_WITH_UNIT(LENGTH_MEASURE(0.001),#11560,
'DISTANCE_ACCURACY_VALUE',
'Maximum model space distance between geometric entities at asserted c
onnectivities');
#11507=UNCERTAINTY_MEASURE_WITH_UNIT(LENGTH_MEASURE(0.001),#11560,
'DISTANCE_ACCURACY_VALUE',
'Maximum model space distance between geometric entities at asserted c
onnectivities');
#11508=UNCERTAINTY_MEASURE_WITH_UNIT(LENGTH_MEASURE(0.001),#11560,
'DISTANCE_ACCURACY_VALUE',
'Maximum model space distance between geometric entities at asserted c
onnectivities');
#11509=UNCERTAINTY_MEASURE_WITH_UNIT(LENGTH_MEASURE(0.001),#11560,
'DISTANCE_ACCURACY_VALUE',
'Maximum model space distance between geometric entities at asserted c
onnectivities');
#11510=UNCERTAINTY_MEASURE_WITH_UNIT(LENGTH_MEASURE(0.001),#11560,
'DISTANCE_ACCURACY_VALUE',
'Maximum model space distance between geometric entities at asserted c
onnectivities');
#11511=UNCERTAINTY_MEASURE_WITH_UNIT(LENGTH_MEASURE(0.001),#11560,
'DISTANCE_ACCURACY_VALUE',
'Maximum model space distance between geometric entities at asserted c
onnectivities');
#11512=UNCERTAINTY_MEASURE_WITH_UNIT(LENGTH_MEASURE(0.001),#11560,
'DISTANCE_ACCURACY_VALUE',
'Maximum model space distance between geometric entities at asserted c
onnectivities');
#11513=UNCERTAINTY_MEASURE_WITH_UNIT(LENGTH_MEASURE(0.001),#11560,
'DISTANCE_ACCURACY_VALUE',
'Maximum model space distance between geometric entities at asserted c
onnectivities');
#11514=UNCERTAINTY_MEASURE_WITH_UNIT(LENGTH_MEASURE(0.001),#11560,
'DISTANCE_ACCURACY_VALUE',
'Maximum model space distance between geometric entities at asserted c
onnectivities');
#11515=UNCERTAINTY_MEASURE_WITH_UNIT(LENGTH_MEASURE(0.001),#11560,
'DISTANCE_ACCURACY_VALUE',
'Maximum model space distance between geometric entities at asserted c
onnectivities');
#11516=UNCERTAINTY_MEASURE_WITH_UNIT(LENGTH_MEASURE(0.001),#11560,
'DISTANCE_ACCURACY_VALUE',
'Maximum model space distance between geometric entities at asserted c
onnectivities');
#11517=UNCERTAINTY_MEASURE_WITH_UNIT(LENGTH_MEASURE(0.001),#11560,
'DISTANCE_ACCURACY_VALUE',
'Maximum model space distance between geometric entities at asserted c
onnectivities');
#11518=UNCERTAINTY_MEASURE_WITH_UNIT(LENGTH_MEASURE(0.001),#11560,
'DISTANCE_ACCURACY_VALUE',
'Maximum model space distance between geometric entities at asserted c
onnectivities');
#11519=UNCERTAINTY_MEASURE_WITH_UNIT(LENGTH_MEASURE(0.001),#11560,
'DISTANCE_ACCURACY_VALUE',
'Maximum model space distance between geometric entities at asserted c
onnectivities');
#11520=UNCERTAINTY_MEASURE_WITH_UNIT(LENGTH_MEASURE(0.001),#11560,
'DISTANCE_ACCURACY_VALUE',
'Maximum model space distance between geometric entities at asserted c
onnectivities');
#11521=UNCERTAINTY_MEASURE_WITH_UNIT(LENGTH_MEASURE(0.001),#11560,
'DISTANCE_ACCURACY_VALUE',
'Maximum model space distance between geometric entities at asserted c
onnectivities');
#11522=UNCERTAINTY_MEASURE_WITH_UNIT(LENGTH_MEASURE(0.001),#11560,
'DISTANCE_ACCURACY_VALUE',
'Maximum model space distance between geometric entities at asserted c
onnectivities');
#11523=(
GEOMETRIC_REPRESENTATION_CONTEXT(3)
GLOBAL_UNCERTAINTY_ASSIGNED_CONTEXT((#11486))
GLOBAL_UNIT_ASSIGNED_CONTEXT((#11560,#11562,#11563))
REPRESENTATION_CONTEXT('','3D')
);
#11524=(
GEOMETRIC_REPRESENTATION_CONTEXT(3)
GLOBAL_UNCERTAINTY_ASSIGNED_CONTEXT((#11487))
GLOBAL_UNIT_ASSIGNED_CONTEXT((#11560,#11562,#11563))
REPRESENTATION_CONTEXT('','3D')
);
#11525=(
GEOMETRIC_REPRESENTATION_CONTEXT(3)
GLOBAL_UNCERTAINTY_ASSIGNED_CONTEXT((#11488))
GLOBAL_UNIT_ASSIGNED_CONTEXT((#11560,#11562,#11563))
REPRESENTATION_CONTEXT('','3D')
);
#11526=(
GEOMETRIC_REPRESENTATION_CONTEXT(3)
GLOBAL_UNCERTAINTY_ASSIGNED_CONTEXT((#11489))
GLOBAL_UNIT_ASSIGNED_CONTEXT((#11560,#11562,#11563))
REPRESENTATION_CONTEXT('','3D')
);
#11527=(
GEOMETRIC_REPRESENTATION_CONTEXT(3)
GLOBAL_UNCERTAINTY_ASSIGNED_CONTEXT((#11490))
GLOBAL_UNIT_ASSIGNED_CONTEXT((#11560,#11562,#11563))
REPRESENTATION_CONTEXT('','3D')
);
#11528=(
GEOMETRIC_REPRESENTATION_CONTEXT(3)
GLOBAL_UNCERTAINTY_ASSIGNED_CONTEXT((#11491))
GLOBAL_UNIT_ASSIGNED_CONTEXT((#11560,#11562,#11563))
REPRESENTATION_CONTEXT('','3D')
);
#11529=(
GEOMETRIC_REPRESENTATION_CONTEXT(3)
GLOBAL_UNCERTAINTY_ASSIGNED_CONTEXT((#11492))
GLOBAL_UNIT_ASSIGNED_CONTEXT((#11560,#11562,#11563))
REPRESENTATION_CONTEXT('','3D')
);
#11530=(
GEOMETRIC_REPRESENTATION_CONTEXT(3)
GLOBAL_UNCERTAINTY_ASSIGNED_CONTEXT((#11493))
GLOBAL_UNIT_ASSIGNED_CONTEXT((#11560,#11562,#11563))
REPRESENTATION_CONTEXT('','3D')
);
#11531=(
GEOMETRIC_REPRESENTATION_CONTEXT(3)
GLOBAL_UNCERTAINTY_ASSIGNED_CONTEXT((#11494))
GLOBAL_UNIT_ASSIGNED_CONTEXT((#11560,#11562,#11563))
REPRESENTATION_CONTEXT('','3D')
);
#11532=(
GEOMETRIC_REPRESENTATION_CONTEXT(3)
GLOBAL_UNCERTAINTY_ASSIGNED_CONTEXT((#11495))
GLOBAL_UNIT_ASSIGNED_CONTEXT((#11560,#11562,#11563))
REPRESENTATION_CONTEXT('','3D')
);
#11533=(
GEOMETRIC_REPRESENTATION_CONTEXT(3)
GLOBAL_UNCERTAINTY_ASSIGNED_CONTEXT((#11496))
GLOBAL_UNIT_ASSIGNED_CONTEXT((#11560,#11562,#11563))
REPRESENTATION_CONTEXT('','3D')
);
#11534=(
GEOMETRIC_REPRESENTATION_CONTEXT(3)
GLOBAL_UNCERTAINTY_ASSIGNED_CONTEXT((#11497))
GLOBAL_UNIT_ASSIGNED_CONTEXT((#11560,#11562,#11563))
REPRESENTATION_CONTEXT('','3D')
);
#11535=(
GEOMETRIC_REPRESENTATION_CONTEXT(3)
GLOBAL_UNCERTAINTY_ASSIGNED_CONTEXT((#11498))
GLOBAL_UNIT_ASSIGNED_CONTEXT((#11560,#11562,#11563))
REPRESENTATION_CONTEXT('','3D')
);
#11536=(
GEOMETRIC_REPRESENTATION_CONTEXT(3)
GLOBAL_UNCERTAINTY_ASSIGNED_CONTEXT((#11499))
GLOBAL_UNIT_ASSIGNED_CONTEXT((#11560,#11562,#11563))
REPRESENTATION_CONTEXT('','3D')
);
#11537=(
GEOMETRIC_REPRESENTATION_CONTEXT(3)
GLOBAL_UNCERTAINTY_ASSIGNED_CONTEXT((#11500))
GLOBAL_UNIT_ASSIGNED_CONTEXT((#11560,#11562,#11563))
REPRESENTATION_CONTEXT('','3D')
);
#11538=(
GEOMETRIC_REPRESENTATION_CONTEXT(3)
GLOBAL_UNCERTAINTY_ASSIGNED_CONTEXT((#11501))
GLOBAL_UNIT_ASSIGNED_CONTEXT((#11560,#11562,#11563))
REPRESENTATION_CONTEXT('','3D')
);
#11539=(
GEOMETRIC_REPRESENTATION_CONTEXT(3)
GLOBAL_UNCERTAINTY_ASSIGNED_CONTEXT((#11502))
GLOBAL_UNIT_ASSIGNED_CONTEXT((#11560,#11562,#11563))
REPRESENTATION_CONTEXT('','3D')
);
#11540=(
GEOMETRIC_REPRESENTATION_CONTEXT(3)
GLOBAL_UNCERTAINTY_ASSIGNED_CONTEXT((#11503))
GLOBAL_UNIT_ASSIGNED_CONTEXT((#11560,#11562,#11563))
REPRESENTATION_CONTEXT('','3D')
);
#11541=(
GEOMETRIC_REPRESENTATION_CONTEXT(3)
GLOBAL_UNCERTAINTY_ASSIGNED_CONTEXT((#11504))
GLOBAL_UNIT_ASSIGNED_CONTEXT((#11560,#11562,#11563))
REPRESENTATION_CONTEXT('','3D')
);
#11542=(
GEOMETRIC_REPRESENTATION_CONTEXT(3)
GLOBAL_UNCERTAINTY_ASSIGNED_CONTEXT((#11505))
GLOBAL_UNIT_ASSIGNED_CONTEXT((#11560,#11562,#11563))
REPRESENTATION_CONTEXT('','3D')
);
#11543=(
GEOMETRIC_REPRESENTATION_CONTEXT(3)
GLOBAL_UNCERTAINTY_ASSIGNED_CONTEXT((#11506))
GLOBAL_UNIT_ASSIGNED_CONTEXT((#11560,#11562,#11563))
REPRESENTATION_CONTEXT('','3D')
);
#11544=(
GEOMETRIC_REPRESENTATION_CONTEXT(3)
GLOBAL_UNCERTAINTY_ASSIGNED_CONTEXT((#11507))
GLOBAL_UNIT_ASSIGNED_CONTEXT((#11560,#11562,#11563))
REPRESENTATION_CONTEXT('','3D')
);
#11545=(
GEOMETRIC_REPRESENTATION_CONTEXT(3)
GLOBAL_UNCERTAINTY_ASSIGNED_CONTEXT((#11508))
GLOBAL_UNIT_ASSIGNED_CONTEXT((#11560,#11562,#11563))
REPRESENTATION_CONTEXT('','3D')
);
#11546=(
GEOMETRIC_REPRESENTATION_CONTEXT(3)
GLOBAL_UNCERTAINTY_ASSIGNED_CONTEXT((#11509))
GLOBAL_UNIT_ASSIGNED_CONTEXT((#11560,#11562,#11563))
REPRESENTATION_CONTEXT('','3D')
);
#11547=(
GEOMETRIC_REPRESENTATION_CONTEXT(3)
GLOBAL_UNCERTAINTY_ASSIGNED_CONTEXT((#11510))
GLOBAL_UNIT_ASSIGNED_CONTEXT((#11560,#11562,#11563))
REPRESENTATION_CONTEXT('','3D')
);
#11548=(
GEOMETRIC_REPRESENTATION_CONTEXT(3)
GLOBAL_UNCERTAINTY_ASSIGNED_CONTEXT((#11511))
GLOBAL_UNIT_ASSIGNED_CONTEXT((#11560,#11562,#11563))
REPRESENTATION_CONTEXT('','3D')
);
#11549=(
GEOMETRIC_REPRESENTATION_CONTEXT(3)
GLOBAL_UNCERTAINTY_ASSIGNED_CONTEXT((#11512))
GLOBAL_UNIT_ASSIGNED_CONTEXT((#11560,#11562,#11563))
REPRESENTATION_CONTEXT('','3D')
);
#11550=(
GEOMETRIC_REPRESENTATION_CONTEXT(3)
GLOBAL_UNCERTAINTY_ASSIGNED_CONTEXT((#11513))
GLOBAL_UNIT_ASSIGNED_CONTEXT((#11560,#11562,#11563))
REPRESENTATION_CONTEXT('','3D')
);
#11551=(
GEOMETRIC_REPRESENTATION_CONTEXT(3)
GLOBAL_UNCERTAINTY_ASSIGNED_CONTEXT((#11514))
GLOBAL_UNIT_ASSIGNED_CONTEXT((#11560,#11562,#11563))
REPRESENTATION_CONTEXT('','3D')
);
#11552=(
GEOMETRIC_REPRESENTATION_CONTEXT(3)
GLOBAL_UNCERTAINTY_ASSIGNED_CONTEXT((#11515))
GLOBAL_UNIT_ASSIGNED_CONTEXT((#11560,#11562,#11563))
REPRESENTATION_CONTEXT('','3D')
);
#11553=(
GEOMETRIC_REPRESENTATION_CONTEXT(3)
GLOBAL_UNCERTAINTY_ASSIGNED_CONTEXT((#11516))
GLOBAL_UNIT_ASSIGNED_CONTEXT((#11560,#11562,#11563))
REPRESENTATION_CONTEXT('','3D')
);
#11554=(
GEOMETRIC_REPRESENTATION_CONTEXT(3)
GLOBAL_UNCERTAINTY_ASSIGNED_CONTEXT((#11517))
GLOBAL_UNIT_ASSIGNED_CONTEXT((#11560,#11562,#11563))
REPRESENTATION_CONTEXT('','3D')
);
#11555=(
GEOMETRIC_REPRESENTATION_CONTEXT(3)
GLOBAL_UNCERTAINTY_ASSIGNED_CONTEXT((#11518))
GLOBAL_UNIT_ASSIGNED_CONTEXT((#11560,#11562,#11563))
REPRESENTATION_CONTEXT('','3D')
);
#11556=(
GEOMETRIC_REPRESENTATION_CONTEXT(3)
GLOBAL_UNCERTAINTY_ASSIGNED_CONTEXT((#11519))
GLOBAL_UNIT_ASSIGNED_CONTEXT((#11560,#11562,#11563))
REPRESENTATION_CONTEXT('','3D')
);
#11557=(
GEOMETRIC_REPRESENTATION_CONTEXT(3)
GLOBAL_UNCERTAINTY_ASSIGNED_CONTEXT((#11520))
GLOBAL_UNIT_ASSIGNED_CONTEXT((#11560,#11562,#11563))
REPRESENTATION_CONTEXT('','3D')
);
#11558=(
GEOMETRIC_REPRESENTATION_CONTEXT(3)
GLOBAL_UNCERTAINTY_ASSIGNED_CONTEXT((#11521))
GLOBAL_UNIT_ASSIGNED_CONTEXT((#11560,#11562,#11563))
REPRESENTATION_CONTEXT('','3D')
);
#11559=(
GEOMETRIC_REPRESENTATION_CONTEXT(3)
GLOBAL_UNCERTAINTY_ASSIGNED_CONTEXT((#11522))
GLOBAL_UNIT_ASSIGNED_CONTEXT((#11560,#11562,#11563))
REPRESENTATION_CONTEXT('','3D')
);
#11560=(
LENGTH_UNIT()
NAMED_UNIT(*)
SI_UNIT(.CENTI.,.METRE.)
);
#11561=(
LENGTH_UNIT()
NAMED_UNIT(*)
SI_UNIT($,.METRE.)
);
#11562=(
NAMED_UNIT(*)
PLANE_ANGLE_UNIT()
SI_UNIT($,.RADIAN.)
);
#11563=(
NAMED_UNIT(*)
SI_UNIT($,.STERADIAN.)
SOLID_ANGLE_UNIT()
);
#11564=SHAPE_DEFINITION_REPRESENTATION(#11600,#11721);
#11565=SHAPE_DEFINITION_REPRESENTATION(#11601,#11722);
#11566=SHAPE_DEFINITION_REPRESENTATION(#11602,#11723);
#11567=SHAPE_DEFINITION_REPRESENTATION(#11603,#11724);
#11568=SHAPE_DEFINITION_REPRESENTATION(#11604,#11725);
#11569=SHAPE_DEFINITION_REPRESENTATION(#11605,#11726);
#11570=SHAPE_DEFINITION_REPRESENTATION(#11606,#11727);
#11571=SHAPE_DEFINITION_REPRESENTATION(#11607,#11728);
#11572=SHAPE_DEFINITION_REPRESENTATION(#11608,#11729);
#11573=SHAPE_DEFINITION_REPRESENTATION(#11609,#11730);
#11574=SHAPE_DEFINITION_REPRESENTATION(#11610,#11731);
#11575=SHAPE_DEFINITION_REPRESENTATION(#11611,#11732);
#11576=SHAPE_DEFINITION_REPRESENTATION(#11612,#11733);
#11577=SHAPE_DEFINITION_REPRESENTATION(#11613,#11734);
#11578=SHAPE_DEFINITION_REPRESENTATION(#11614,#11735);
#11579=SHAPE_DEFINITION_REPRESENTATION(#11615,#11736);
#11580=SHAPE_DEFINITION_REPRESENTATION(#11616,#11737);
#11581=SHAPE_DEFINITION_REPRESENTATION(#11617,#11738);
#11582=SHAPE_DEFINITION_REPRESENTATION(#11618,#11739);
#11583=SHAPE_DEFINITION_REPRESENTATION(#11619,#11740);
#11584=SHAPE_DEFINITION_REPRESENTATION(#11620,#11741);
#11585=SHAPE_DEFINITION_REPRESENTATION(#11621,#11742);
#11586=SHAPE_DEFINITION_REPRESENTATION(#11622,#11743);
#11587=SHAPE_DEFINITION_REPRESENTATION(#11623,#11744);
#11588=SHAPE_DEFINITION_REPRESENTATION(#11626,#11745);
#11589=SHAPE_DEFINITION_REPRESENTATION(#11627,#11746);
#11590=SHAPE_DEFINITION_REPRESENTATION(#11628,#11747);
#11591=SHAPE_DEFINITION_REPRESENTATION(#11702,#11748);
#11592=SHAPE_DEFINITION_REPRESENTATION(#11703,#11749);
#11593=SHAPE_DEFINITION_REPRESENTATION(#11704,#11750);
#11594=SHAPE_DEFINITION_REPRESENTATION(#11705,#11751);
#11595=SHAPE_DEFINITION_REPRESENTATION(#11706,#11752);
#11596=SHAPE_DEFINITION_REPRESENTATION(#11707,#11753);
#11597=SHAPE_DEFINITION_REPRESENTATION(#11708,#11754);
#11598=SHAPE_DEFINITION_REPRESENTATION(#11709,#11755);
#11599=SHAPE_DEFINITION_REPRESENTATION(#11710,#11756);
#11600=PRODUCT_DEFINITION_SHAPE('',$,#11758);
#11601=PRODUCT_DEFINITION_SHAPE('',$,#11759);
#11602=PRODUCT_DEFINITION_SHAPE('',$,#11760);
#11603=PRODUCT_DEFINITION_SHAPE('',$,#11761);
#11604=PRODUCT_DEFINITION_SHAPE('',$,#11762);
#11605=PRODUCT_DEFINITION_SHAPE('',$,#11763);
#11606=PRODUCT_DEFINITION_SHAPE('',$,#11764);
#11607=PRODUCT_DEFINITION_SHAPE('',$,#11765);
#11608=PRODUCT_DEFINITION_SHAPE('',$,#11766);
#11609=PRODUCT_DEFINITION_SHAPE('',$,#11767);
#11610=PRODUCT_DEFINITION_SHAPE('',$,#11768);
#11611=PRODUCT_DEFINITION_SHAPE('',$,#11769);
#11612=PRODUCT_DEFINITION_SHAPE('',$,#11770);
#11613=PRODUCT_DEFINITION_SHAPE('',$,#11771);
#11614=PRODUCT_DEFINITION_SHAPE('',$,#11772);
#11615=PRODUCT_DEFINITION_SHAPE('',$,#11773);
#11616=PRODUCT_DEFINITION_SHAPE('',$,#11774);
#11617=PRODUCT_DEFINITION_SHAPE('',$,#11775);
#11618=PRODUCT_DEFINITION_SHAPE('',$,#11776);
#11619=PRODUCT_DEFINITION_SHAPE('',$,#11777);
#11620=PRODUCT_DEFINITION_SHAPE('',$,#11778);
#11621=PRODUCT_DEFINITION_SHAPE('',$,#11779);
#11622=PRODUCT_DEFINITION_SHAPE('',$,#11780);
#11623=PRODUCT_DEFINITION_SHAPE('',$,#11781);
#11624=PRODUCT_DEFINITION_SHAPE($,$,#278);
#11625=PRODUCT_DEFINITION_SHAPE($,$,#279);
#11626=PRODUCT_DEFINITION_SHAPE('',$,#11782);
#11627=PRODUCT_DEFINITION_SHAPE('',$,#11783);
#11628=PRODUCT_DEFINITION_SHAPE('',$,#11784);
#11629=PRODUCT_DEFINITION_SHAPE($,$,#280);
#11630=PRODUCT_DEFINITION_SHAPE($,$,#281);
#11631=PRODUCT_DEFINITION_SHAPE($,$,#282);
#11632=PRODUCT_DEFINITION_SHAPE($,$,#283);
#11633=PRODUCT_DEFINITION_SHAPE($,$,#284);
#11634=PRODUCT_DEFINITION_SHAPE($,$,#285);
#11635=PRODUCT_DEFINITION_SHAPE($,$,#286);
#11636=PRODUCT_DEFINITION_SHAPE($,$,#287);
#11637=PRODUCT_DEFINITION_SHAPE($,$,#288);
#11638=PRODUCT_DEFINITION_SHAPE($,$,#289);
#11639=PRODUCT_DEFINITION_SHAPE($,$,#290);
#11640=PRODUCT_DEFINITION_SHAPE($,$,#291);
#11641=PRODUCT_DEFINITION_SHAPE($,$,#292);
#11642=PRODUCT_DEFINITION_SHAPE($,$,#293);
#11643=PRODUCT_DEFINITION_SHAPE($,$,#294);
#11644=PRODUCT_DEFINITION_SHAPE($,$,#295);
#11645=PRODUCT_DEFINITION_SHAPE($,$,#296);
#11646=PRODUCT_DEFINITION_SHAPE($,$,#297);
#11647=PRODUCT_DEFINITION_SHAPE($,$,#298);
#11648=PRODUCT_DEFINITION_SHAPE($,$,#299);
#11649=PRODUCT_DEFINITION_SHAPE($,$,#300);
#11650=PRODUCT_DEFINITION_SHAPE($,$,#301);
#11651=PRODUCT_DEFINITION_SHAPE($,$,#302);
#11652=PRODUCT_DEFINITION_SHAPE($,$,#303);
#11653=PRODUCT_DEFINITION_SHAPE($,$,#304);
#11654=PRODUCT_DEFINITION_SHAPE($,$,#305);
#11655=PRODUCT_DEFINITION_SHAPE($,$,#306);
#11656=PRODUCT_DEFINITION_SHAPE($,$,#307);
#11657=PRODUCT_DEFINITION_SHAPE($,$,#308);
#11658=PRODUCT_DEFINITION_SHAPE($,$,#309);
#11659=PRODUCT_DEFINITION_SHAPE($,$,#310);
#11660=PRODUCT_DEFINITION_SHAPE($,$,#311);
#11661=PRODUCT_DEFINITION_SHAPE($,$,#312);
#11662=PRODUCT_DEFINITION_SHAPE($,$,#313);
#11663=PRODUCT_DEFINITION_SHAPE($,$,#314);
#11664=PRODUCT_DEFINITION_SHAPE($,$,#315);
#11665=PRODUCT_DEFINITION_SHAPE($,$,#316);
#11666=PRODUCT_DEFINITION_SHAPE($,$,#317);
#11667=PRODUCT_DEFINITION_SHAPE($,$,#318);
#11668=PRODUCT_DEFINITION_SHAPE($,$,#319);
#11669=PRODUCT_DEFINITION_SHAPE($,$,#320);
#11670=PRODUCT_DEFINITION_SHAPE($,$,#321);
#11671=PRODUCT_DEFINITION_SHAPE($,$,#322);
#11672=PRODUCT_DEFINITION_SHAPE($,$,#323);
#11673=PRODUCT_DEFINITION_SHAPE($,$,#324);
#11674=PRODUCT_DEFINITION_SHAPE($,$,#325);
#11675=PRODUCT_DEFINITION_SHAPE($,$,#326);
#11676=PRODUCT_DEFINITION_SHAPE($,$,#327);
#11677=PRODUCT_DEFINITION_SHAPE($,$,#328);
#11678=PRODUCT_DEFINITION_SHAPE($,$,#329);
#11679=PRODUCT_DEFINITION_SHAPE($,$,#330);
#11680=PRODUCT_DEFINITION_SHAPE($,$,#331);
#11681=PRODUCT_DEFINITION_SHAPE($,$,#332);
#11682=PRODUCT_DEFINITION_SHAPE($,$,#333);
#11683=PRODUCT_DEFINITION_SHAPE($,$,#334);
#11684=PRODUCT_DEFINITION_SHAPE($,$,#335);
#11685=PRODUCT_DEFINITION_SHAPE($,$,#336);
#11686=PRODUCT_DEFINITION_SHAPE($,$,#337);
#11687=PRODUCT_DEFINITION_SHAPE($,$,#338);
#11688=PRODUCT_DEFINITION_SHAPE($,$,#339);
#11689=PRODUCT_DEFINITION_SHAPE($,$,#340);
#11690=PRODUCT_DEFINITION_SHAPE($,$,#341);
#11691=PRODUCT_DEFINITION_SHAPE($,$,#342);
#11692=PRODUCT_DEFINITION_SHAPE($,$,#343);
#11693=PRODUCT_DEFINITION_SHAPE($,$,#344);
#11694=PRODUCT_DEFINITION_SHAPE($,$,#345);
#11695=PRODUCT_DEFINITION_SHAPE($,$,#346);
#11696=PRODUCT_DEFINITION_SHAPE($,$,#347);
#11697=PRODUCT_DEFINITION_SHAPE($,$,#348);
#11698=PRODUCT_DEFINITION_SHAPE($,$,#349);
#11699=PRODUCT_DEFINITION_SHAPE($,$,#350);
#11700=PRODUCT_DEFINITION_SHAPE($,$,#351);
#11701=PRODUCT_DEFINITION_SHAPE($,$,#352);
#11702=PRODUCT_DEFINITION_SHAPE('',$,#11785);
#11703=PRODUCT_DEFINITION_SHAPE('',$,#11786);
#11704=PRODUCT_DEFINITION_SHAPE('',$,#11787);
#11705=PRODUCT_DEFINITION_SHAPE('',$,#11788);
#11706=PRODUCT_DEFINITION_SHAPE('',$,#11789);
#11707=PRODUCT_DEFINITION_SHAPE('',$,#11790);
#11708=PRODUCT_DEFINITION_SHAPE('',$,#11791);
#11709=PRODUCT_DEFINITION_SHAPE('',$,#11792);
#11710=PRODUCT_DEFINITION_SHAPE('',$,#11793);
#11711=PRODUCT_DEFINITION_SHAPE($,$,#353);
#11712=PRODUCT_DEFINITION_SHAPE($,$,#354);
#11713=PRODUCT_DEFINITION_SHAPE($,$,#355);
#11714=PRODUCT_DEFINITION_SHAPE($,$,#356);
#11715=PRODUCT_DEFINITION_SHAPE($,$,#357);
#11716=PRODUCT_DEFINITION_SHAPE($,$,#358);
#11717=PRODUCT_DEFINITION_SHAPE($,$,#359);
#11718=PRODUCT_DEFINITION_SHAPE($,$,#360);
#11719=PRODUCT_DEFINITION_SHAPE($,$,#361);
#11720=PRODUCT_DEFINITION_SHAPE($,$,#362);
#11721=SHAPE_REPRESENTATION('',(#6713,#7369,#7370),#11523);
#11722=SHAPE_REPRESENTATION('',(#6714,#7158,#7159,#7160,#7161,#7162,#7163,
#7164,#7165,#7166,#7167,#7168,#7169,#7170,#7171,#7172,#7173,#7174,#7175,
#7176,#7177,#7178,#7179,#7180,#7181,#7182,#7183,#7184,#7185,#7186,#7187,
#7188,#7189,#7190,#7191,#7192,#7193,#7194,#7195,#7196,#7197,#7198,#7199,
#7200,#7201,#7202,#7203,#7204,#7205,#7206,#7207,#7208,#7209,#7210,#7211,
#7212,#7213,#7214,#7215,#7216,#7217,#7218,#7219,#7220,#7221,#7222,#7223,
#7224,#7225,#7226,#7227,#7228,#7229,#7230),#11524);
#11723=SHAPE_REPRESENTATION('',(#6715),#11525);
#11724=SHAPE_REPRESENTATION('',(#6758),#11526);
#11725=SHAPE_REPRESENTATION('',(#6765),#11527);
#11726=SHAPE_REPRESENTATION('',(#6772),#11528);
#11727=SHAPE_REPRESENTATION('',(#6779),#11529);
#11728=SHAPE_REPRESENTATION('',(#6786),#11530);
#11729=SHAPE_REPRESENTATION('',(#6816),#11531);
#11730=SHAPE_REPRESENTATION('',(#6825),#11532);
#11731=SHAPE_REPRESENTATION('',(#6834),#11533);
#11732=SHAPE_REPRESENTATION('',(#6843),#11534);
#11733=SHAPE_REPRESENTATION('',(#6852),#11535);
#11734=SHAPE_REPRESENTATION('',(#6882),#11536);
#11735=SHAPE_REPRESENTATION('',(#6891),#11537);
#11736=SHAPE_REPRESENTATION('',(#6900),#11538);
#11737=SHAPE_REPRESENTATION('',(#6909),#11539);
#11738=SHAPE_REPRESENTATION('',(#6918),#11540);
#11739=SHAPE_REPRESENTATION('',(#6968),#11541);
#11740=SHAPE_REPRESENTATION('',(#6989),#11542);
#11741=SHAPE_REPRESENTATION('',(#7013),#11543);
#11742=SHAPE_REPRESENTATION('',(#7037,#7105,#7106),#11544);
#11743=SHAPE_REPRESENTATION('',(#7038),#11545);
#11744=SHAPE_REPRESENTATION('',(#7077),#11546);
#11745=SHAPE_REPRESENTATION('',(#7107),#11547);
#11746=SHAPE_REPRESENTATION('',(#7133),#11548);
#11747=SHAPE_REPRESENTATION('',(#7142),#11549);
#11748=SHAPE_REPRESENTATION('',(#7231,#7361,#7362,#7363,#7364,#7365,#7366,
#7367,#7368),#11550);
#11749=SHAPE_REPRESENTATION('',(#7232),#11551);
#11750=SHAPE_REPRESENTATION('',(#7253),#11552);
#11751=SHAPE_REPRESENTATION('',(#7262),#11553);
#11752=SHAPE_REPRESENTATION('',(#7271),#11554);
#11753=SHAPE_REPRESENTATION('',(#7283),#11555);
#11754=SHAPE_REPRESENTATION('',(#7295),#11556);
#11755=SHAPE_REPRESENTATION('',(#7333),#11557);
#11756=SHAPE_REPRESENTATION('',(#7344),#11558);
#11757=PRODUCT_DEFINITION_CONTEXT('part definition',#11867,'design');
#11758=PRODUCT_DEFINITION('PAT-031',
'PAT-031',#11794,#11757);
#11759=PRODUCT_DEFINITION('Extrusion support frame',
'Extrusion support frame',#11795,#11757);
#11760=PRODUCT_DEFINITION('Base plate','Base plate',#11796,#11757);
#11761=PRODUCT_DEFINITION('Bonded foot pad','Bonded foot pad',#11797,#11757);
#11762=PRODUCT_DEFINITION('Bonded foot pad (1)','Bonded foot pad (1)',#11798,
#11757);
#11763=PRODUCT_DEFINITION('Bonded foot pad (2)','Bonded foot pad (2)',#11799,
#11757);
#11764=PRODUCT_DEFINITION('Bonded foot pad (3)','Bonded foot pad (3)',#11800,
#11757);
#11765=PRODUCT_DEFINITION('Flange adapter','Flange adapter',#11801,#11757);
#11766=PRODUCT_DEFINITION('Flange hole reducer','Flange hole reducer',#11802,
#11757);
#11767=PRODUCT_DEFINITION('Flange hole reducer (1)',
'Flange hole reducer (1)',#11803,#11757);
#11768=PRODUCT_DEFINITION('Flange hole reducer (2)',
'Flange hole reducer (2)',#11804,#11757);
#11769=PRODUCT_DEFINITION('Flange hole reducer (3)',
'Flange hole reducer (3)',#11805,#11757);
#11770=PRODUCT_DEFINITION('Flange adapter (1)','Flange adapter (1)',#11806,
#11757);
#11771=PRODUCT_DEFINITION('Flange hole reducer (4)',
'Flange hole reducer (4)',#11807,#11757);
#11772=PRODUCT_DEFINITION('Flange hole reducer (5)',
'Flange hole reducer (5)',#11808,#11757);
#11773=PRODUCT_DEFINITION('Flange hole reducer (6)',
'Flange hole reducer (6)',#11809,#11757);
#11774=PRODUCT_DEFINITION('Flange hole reducer (7)',
'Flange hole reducer (7)',#11810,#11757);
#11775=PRODUCT_DEFINITION('Slotted Extrusion - 20 x 20 x 200 mm',
'Slotted Extrusion - 20 x 20 x 200 mm',#11811,#11757);
#11776=PRODUCT_DEFINITION('Captive slot nut','Captive slot nut',#11812,
#11757);
#11777=PRODUCT_DEFINITION('M5x17 screw','M5x17 screw',#11813,#11757);
#11778=PRODUCT_DEFINITION('M6x18 mounting screw','M6x18 mounting screw',
#11814,#11757);
#11779=PRODUCT_DEFINITION('Square Flange Bearing - 12 mm Bore',
'Square Flange Bearing - 12 mm Bore',#11815,#11757);
#11780=PRODUCT_DEFINITION('Housing','Housing',#11816,#11757);
#11781=PRODUCT_DEFINITION('Insert bearing','Insert bearing',#11817,#11757);
#11782=PRODUCT_DEFINITION('Cap Screw - M8x30','Cap Screw - M8x30',#11818,
#11757);
#11783=PRODUCT_DEFINITION('Flat Washer - M8','Flat Washer - M8',#11819,
#11757);
#11784=PRODUCT_DEFINITION('Hex Nut - M8','Hex Nut - M8',#11820,#11757);
#11785=PRODUCT_DEFINITION('Shaft and axial retention',
'Shaft and axial retention',#11821,#11757);
#11786=PRODUCT_DEFINITION('Shaft','Shaft',#11822,#11757);
#11787=PRODUCT_DEFINITION('Rear thrust spacer','Rear thrust spacer',#11823,
#11757);
#11788=PRODUCT_DEFINITION('Front thrust spacer','Front thrust spacer',#11824,
#11757);
#11789=PRODUCT_DEFINITION('Adjustment nut','Adjustment nut',#11825,#11757);
#11790=PRODUCT_DEFINITION('Jam nut','Jam nut',#11826,#11757);
#11791=PRODUCT_DEFINITION('Drive hub','Drive hub',#11827,#11757);
#11792=PRODUCT_DEFINITION('Key 4x4x14','Key 4x4x14',#11828,#11757);
#11793=PRODUCT_DEFINITION('Socket Set Screw - M5x8',
'Socket Set Screw - M5x8',#11829,#11757);
#11794=PRODUCT_DEFINITION_FORMATION('',$,#11869);
#11795=PRODUCT_DEFINITION_FORMATION('',$,#11870);
#11796=PRODUCT_DEFINITION_FORMATION('',$,#11871);
#11797=PRODUCT_DEFINITION_FORMATION('',$,#11872);
#11798=PRODUCT_DEFINITION_FORMATION('',$,#11873);
#11799=PRODUCT_DEFINITION_FORMATION('',$,#11874);
#11800=PRODUCT_DEFINITION_FORMATION('',$,#11875);
#11801=PRODUCT_DEFINITION_FORMATION('',$,#11876);
#11802=PRODUCT_DEFINITION_FORMATION('',$,#11877);
#11803=PRODUCT_DEFINITION_FORMATION('',$,#11878);
#11804=PRODUCT_DEFINITION_FORMATION('',$,#11879);
#11805=PRODUCT_DEFINITION_FORMATION('',$,#11880);
#11806=PRODUCT_DEFINITION_FORMATION('',$,#11881);
#11807=PRODUCT_DEFINITION_FORMATION('',$,#11882);
#11808=PRODUCT_DEFINITION_FORMATION('',$,#11883);
#11809=PRODUCT_DEFINITION_FORMATION('',$,#11884);
#11810=PRODUCT_DEFINITION_FORMATION('',$,#11885);
#11811=PRODUCT_DEFINITION_FORMATION('',$,#11886);
#11812=PRODUCT_DEFINITION_FORMATION('',$,#11887);
#11813=PRODUCT_DEFINITION_FORMATION('',$,#11888);
#11814=PRODUCT_DEFINITION_FORMATION('',$,#11889);
#11815=PRODUCT_DEFINITION_FORMATION('',$,#11890);
#11816=PRODUCT_DEFINITION_FORMATION('',$,#11891);
#11817=PRODUCT_DEFINITION_FORMATION('',$,#11892);
#11818=PRODUCT_DEFINITION_FORMATION('',$,#11893);
#11819=PRODUCT_DEFINITION_FORMATION('',$,#11894);
#11820=PRODUCT_DEFINITION_FORMATION('',$,#11895);
#11821=PRODUCT_DEFINITION_FORMATION('',$,#11896);
#11822=PRODUCT_DEFINITION_FORMATION('',$,#11897);
#11823=PRODUCT_DEFINITION_FORMATION('',$,#11898);
#11824=PRODUCT_DEFINITION_FORMATION('',$,#11899);
#11825=PRODUCT_DEFINITION_FORMATION('',$,#11900);
#11826=PRODUCT_DEFINITION_FORMATION('',$,#11901);
#11827=PRODUCT_DEFINITION_FORMATION('',$,#11902);
#11828=PRODUCT_DEFINITION_FORMATION('',$,#11903);
#11829=PRODUCT_DEFINITION_FORMATION('',$,#11904);
#11830=PRODUCT_RELATED_PRODUCT_CATEGORY('PAT-031','PAT-031',(#11869));
#11831=PRODUCT_RELATED_PRODUCT_CATEGORY('Extrusion support frame',
'Extrusion support frame',(#11870));
#11832=PRODUCT_RELATED_PRODUCT_CATEGORY('Base plate','Base plate',(#11871));
#11833=PRODUCT_RELATED_PRODUCT_CATEGORY('Bonded foot pad',
'Bonded foot pad',(#11872));
#11834=PRODUCT_RELATED_PRODUCT_CATEGORY('Bonded foot pad (1)',
'Bonded foot pad (1)',(#11873));
#11835=PRODUCT_RELATED_PRODUCT_CATEGORY('Bonded foot pad (2)',
'Bonded foot pad (2)',(#11874));
#11836=PRODUCT_RELATED_PRODUCT_CATEGORY('Bonded foot pad (3)',
'Bonded foot pad (3)',(#11875));
#11837=PRODUCT_RELATED_PRODUCT_CATEGORY('Flange adapter',
'Flange adapter',(#11876));
#11838=PRODUCT_RELATED_PRODUCT_CATEGORY('Flange hole reducer',
'Flange hole reducer',(#11877));
#11839=PRODUCT_RELATED_PRODUCT_CATEGORY('Flange hole reducer (1)',
'Flange hole reducer (1)',(#11878));
#11840=PRODUCT_RELATED_PRODUCT_CATEGORY('Flange hole reducer (2)',
'Flange hole reducer (2)',(#11879));
#11841=PRODUCT_RELATED_PRODUCT_CATEGORY('Flange hole reducer (3)',
'Flange hole reducer (3)',(#11880));
#11842=PRODUCT_RELATED_PRODUCT_CATEGORY('Flange adapter (1)',
'Flange adapter (1)',(#11881));
#11843=PRODUCT_RELATED_PRODUCT_CATEGORY('Flange hole reducer (4)',
'Flange hole reducer (4)',(#11882));
#11844=PRODUCT_RELATED_PRODUCT_CATEGORY('Flange hole reducer (5)',
'Flange hole reducer (5)',(#11883));
#11845=PRODUCT_RELATED_PRODUCT_CATEGORY('Flange hole reducer (6)',
'Flange hole reducer (6)',(#11884));
#11846=PRODUCT_RELATED_PRODUCT_CATEGORY('Flange hole reducer (7)',
'Flange hole reducer (7)',(#11885));
#11847=PRODUCT_RELATED_PRODUCT_CATEGORY(
'Slotted Extrusion - 20 x 20 x 200 mm',
'Slotted Extrusion - 20 x 20 x 200 mm',(#11886));
#11848=PRODUCT_RELATED_PRODUCT_CATEGORY('Captive slot nut',
'Captive slot nut',(#11887));
#11849=PRODUCT_RELATED_PRODUCT_CATEGORY('M5x17 screw','M5x17 screw',(#11888));
#11850=PRODUCT_RELATED_PRODUCT_CATEGORY('M6x18 mounting screw',
'M6x18 mounting screw',(#11889));
#11851=PRODUCT_RELATED_PRODUCT_CATEGORY(
'Square Flange Bearing - 12 mm Bore',
'Square Flange Bearing - 12 mm Bore',(#11890));
#11852=PRODUCT_RELATED_PRODUCT_CATEGORY('Housing','Housing',(#11891));
#11853=PRODUCT_RELATED_PRODUCT_CATEGORY('Insert bearing',
'Insert bearing',(#11892));
#11854=PRODUCT_RELATED_PRODUCT_CATEGORY('Cap Screw - M8x30',
'Cap Screw - M8x30',(#11893));
#11855=PRODUCT_RELATED_PRODUCT_CATEGORY('Flat Washer - M8',
'Flat Washer - M8',(#11894));
#11856=PRODUCT_RELATED_PRODUCT_CATEGORY('Hex Nut - M8','Hex Nut - M8',(#11895));
#11857=PRODUCT_RELATED_PRODUCT_CATEGORY('Shaft and axial retention',
'Shaft and axial retention',(#11896));
#11858=PRODUCT_RELATED_PRODUCT_CATEGORY('Shaft','Shaft',(#11897));
#11859=PRODUCT_RELATED_PRODUCT_CATEGORY('Rear thrust spacer',
'Rear thrust spacer',(#11898));
#11860=PRODUCT_RELATED_PRODUCT_CATEGORY('Front thrust spacer',
'Front thrust spacer',(#11899));
#11861=PRODUCT_RELATED_PRODUCT_CATEGORY('Adjustment nut',
'Adjustment nut',(#11900));
#11862=PRODUCT_RELATED_PRODUCT_CATEGORY('Jam nut','Jam nut',(#11901));
#11863=PRODUCT_RELATED_PRODUCT_CATEGORY('Drive hub','Drive hub',(#11902));
#11864=PRODUCT_RELATED_PRODUCT_CATEGORY('Key 4x4x14','Key 4x4x14',(#11903));
#11865=PRODUCT_RELATED_PRODUCT_CATEGORY('Socket Set Screw - M5x8',
'Socket Set Screw - M5x8',(#11904));
#11866=APPLICATION_PROTOCOL_DEFINITION('international standard',
'automotive_design',2009,#11867);
#11867=APPLICATION_CONTEXT(
'Core Data for Automotive Mechanical Design Process');
#11868=PRODUCT_CONTEXT('part definition',#11867,'mechanical');
#11869=PRODUCT('PAT-031','PAT-031',
'PAT-031',(#11868));
#11870=PRODUCT('Extrusion support frame','Extrusion support frame',
'Extrusion support frame',(#11868));
#11871=PRODUCT('Base plate','Base plate','Base plate',(#11868));
#11872=PRODUCT('Bonded foot pad','Bonded foot pad','Bonded foot pad',(#11868));
#11873=PRODUCT('Bonded foot pad (1)','Bonded foot pad (1)',
'Bonded foot pad (1)',(#11868));
#11874=PRODUCT('Bonded foot pad (2)','Bonded foot pad (2)',
'Bonded foot pad (2)',(#11868));
#11875=PRODUCT('Bonded foot pad (3)','Bonded foot pad (3)',
'Bonded foot pad (3)',(#11868));
#11876=PRODUCT('Flange adapter','Flange adapter','Flange adapter',(#11868));
#11877=PRODUCT('Flange hole reducer','Flange hole reducer',
'Flange hole reducer',(#11868));
#11878=PRODUCT('Flange hole reducer (1)','Flange hole reducer (1)',
'Flange hole reducer (1)',(#11868));
#11879=PRODUCT('Flange hole reducer (2)','Flange hole reducer (2)',
'Flange hole reducer (2)',(#11868));
#11880=PRODUCT('Flange hole reducer (3)','Flange hole reducer (3)',
'Flange hole reducer (3)',(#11868));
#11881=PRODUCT('Flange adapter (1)','Flange adapter (1)','Flange adapter (1)',
(#11868));
#11882=PRODUCT('Flange hole reducer (4)','Flange hole reducer (4)',
'Flange hole reducer (4)',(#11868));
#11883=PRODUCT('Flange hole reducer (5)','Flange hole reducer (5)',
'Flange hole reducer (5)',(#11868));
#11884=PRODUCT('Flange hole reducer (6)','Flange hole reducer (6)',
'Flange hole reducer (6)',(#11868));
#11885=PRODUCT('Flange hole reducer (7)','Flange hole reducer (7)',
'Flange hole reducer (7)',(#11868));
#11886=PRODUCT('Slotted Extrusion - 20 x 20 x 200 mm',
'Slotted Extrusion - 20 x 20 x 200 mm',
'Slotted Extrusion - 20 x 20 x 200 mm',(#11868));
#11887=PRODUCT('Captive slot nut','Captive slot nut','Captive slot nut',
(#11868));
#11888=PRODUCT('M5x17 screw','M5x17 screw','M5x17 screw',(#11868));
#11889=PRODUCT('M6x18 mounting screw','M6x18 mounting screw',
'M6x18 mounting screw',(#11868));
#11890=PRODUCT('Square Flange Bearing - 12 mm Bore',
'Square Flange Bearing - 12 mm Bore',
'Square Flange Bearing - 12 mm Bore',(#11868));
#11891=PRODUCT('Housing','Housing','Housing',(#11868));
#11892=PRODUCT('Insert bearing','Insert bearing','Insert bearing',(#11868));
#11893=PRODUCT('Cap Screw - M8x30','Cap Screw - M8x30',
'Cap Screw - M8x30',(#11868));
#11894=PRODUCT('Flat Washer - M8','Flat Washer - M8','Flat Washer - M8',
(#11868));
#11895=PRODUCT('Hex Nut - M8','Hex Nut - M8','Hex Nut - M8',(#11868));
#11896=PRODUCT('Shaft and axial retention','Shaft and axial retention',
'Shaft and axial retention',(#11868));
#11897=PRODUCT('Shaft','Shaft','Shaft',(#11868));
#11898=PRODUCT('Rear thrust spacer','Rear thrust spacer',
'Rear thrust spacer',(#11868));
#11899=PRODUCT('Front thrust spacer','Front thrust spacer',
'Front thrust spacer',(#11868));
#11900=PRODUCT('Adjustment nut','Adjustment nut','Adjustment nut',(#11868));
#11901=PRODUCT('Jam nut','Jam nut','Jam nut',(#11868));
#11902=PRODUCT('Drive hub','Drive hub','Drive hub',(#11868));
#11903=PRODUCT('Key 4x4x14','Key 4x4x14','Key 4x4x14',(#11868));
#11904=PRODUCT('Socket Set Screw - M5x8','Socket Set Screw - M5x8',
'Socket Set Screw - M5x8',(#11868));
#11905=PRESENTATION_STYLE_ASSIGNMENT((#11910));
#11906=PRESENTATION_STYLE_ASSIGNMENT((#11911));
#11907=PRESENTATION_STYLE_ASSIGNMENT((#11912));
#11908=PRESENTATION_STYLE_ASSIGNMENT((#11913));
#11909=PRESENTATION_STYLE_ASSIGNMENT((#11914));
#11910=SURFACE_STYLE_USAGE(.BOTH.,#11915);
#11911=SURFACE_STYLE_USAGE(.BOTH.,#11916);
#11912=SURFACE_STYLE_USAGE(.BOTH.,#11917);
#11913=SURFACE_STYLE_USAGE(.BOTH.,#11918);
#11914=SURFACE_STYLE_USAGE(.BOTH.,#11919);
#11915=SURFACE_SIDE_STYLE('',(#11920));
#11916=SURFACE_SIDE_STYLE('',(#11921));
#11917=SURFACE_SIDE_STYLE('',(#11922));
#11918=SURFACE_SIDE_STYLE('',(#11923));
#11919=SURFACE_SIDE_STYLE('',(#11924));
#11920=SURFACE_STYLE_FILL_AREA(#11925);
#11921=SURFACE_STYLE_FILL_AREA(#11926);
#11922=SURFACE_STYLE_FILL_AREA(#11927);
#11923=SURFACE_STYLE_FILL_AREA(#11928);
#11924=SURFACE_STYLE_FILL_AREA(#11929);
#11925=FILL_AREA_STYLE('Steel - Satin',(#11930));
#11926=FILL_AREA_STYLE('CAD Library Painted - Deep blue',(#11931));
#11927=FILL_AREA_STYLE('CAD Library Painted - Graphite',(#11932));
#11928=FILL_AREA_STYLE('CAD Library Painted - Engineering blue',(#11933));
#11929=FILL_AREA_STYLE('CAD Library Painted - Steel gray',(#11934));
#11930=FILL_AREA_STYLE_COLOUR('Steel - Satin',#11935);
#11931=FILL_AREA_STYLE_COLOUR('CAD Library Painted - Deep blue',#11936);
#11932=FILL_AREA_STYLE_COLOUR('CAD Library Painted - Graphite',#11937);
#11933=FILL_AREA_STYLE_COLOUR('CAD Library Painted - Engineering blue',
#11938);
#11934=FILL_AREA_STYLE_COLOUR('CAD Library Painted - Steel gray',#11939);
#11935=COLOUR_RGB('Steel - Satin',0.627450980392157,0.627450980392157,0.627450980392157);
#11936=COLOUR_RGB('CAD Library Painted - Deep blue',0.0784313725490196,
0.203921568627451,0.349019607843137);
#11937=COLOUR_RGB('CAD Library Painted - Graphite',0.168627450980392,0.192156862745098,
0.231372549019608);
#11938=COLOUR_RGB('CAD Library Painted - Engineering blue',0.12156862745098,
0.356862745098039,0.6);
#11939=COLOUR_RGB('CAD Library Painted - Steel gray',0.592156862745098,
0.631372549019608,0.67843137254902);
#11940=COLOUR_RGB('Dark Blue',0.08,0.2,0.34);
#11941=FILL_AREA_STYLE_COLOUR('',#11940);
#11942=FILL_AREA_STYLE('',(#11941));
#11943=SURFACE_STYLE_FILL_AREA(#11942);
#11944=SURFACE_SIDE_STYLE('',(#11943));
#11945=SURFACE_STYLE_USAGE(.BOTH.,#11944);
#11946=PRESENTATION_STYLE_ASSIGNMENT((#11945));
#11947=COLOUR_RGB('Light Blue',0.38,0.62,0.78);
#11948=FILL_AREA_STYLE_COLOUR('',#11947);
#11949=FILL_AREA_STYLE('',(#11948));
#11950=SURFACE_STYLE_FILL_AREA(#11949);
#11951=SURFACE_SIDE_STYLE('',(#11950));
#11952=SURFACE_STYLE_USAGE(.BOTH.,#11951);
#11953=PRESENTATION_STYLE_ASSIGNMENT((#11952));
#11954=COLOUR_RGB('Sky Blue',0.24,0.69,0.87);
#11955=FILL_AREA_STYLE_COLOUR('',#11954);
#11956=FILL_AREA_STYLE('',(#11955));
#11957=SURFACE_STYLE_FILL_AREA(#11956);
#11958=SURFACE_SIDE_STYLE('',(#11957));
#11959=SURFACE_STYLE_USAGE(.BOTH.,#11958);
#11960=PRESENTATION_STYLE_ASSIGNMENT((#11959));
#11961=COLOUR_RGB('Grey',0.48,0.52,0.57);
#11962=FILL_AREA_STYLE_COLOUR('',#11961);
#11963=FILL_AREA_STYLE('',(#11962));
#11964=SURFACE_STYLE_FILL_AREA(#11963);
#11965=SURFACE_SIDE_STYLE('',(#11964));
#11966=SURFACE_STYLE_USAGE(.BOTH.,#11965);
#11967=PRESENTATION_STYLE_ASSIGNMENT((#11966));
#11968=COLOUR_RGB('Black',0.12,0.14,0.17);
#11969=FILL_AREA_STYLE_COLOUR('',#11968);
#11970=FILL_AREA_STYLE('',(#11969));
#11971=SURFACE_STYLE_FILL_AREA(#11970);
#11972=SURFACE_SIDE_STYLE('',(#11971));
#11973=SURFACE_STYLE_USAGE(.BOTH.,#11972);
#11974=PRESENTATION_STYLE_ASSIGNMENT((#11973));
#11975=COLOUR_RGB('Off White',0.89,0.88,0.83);
#11976=FILL_AREA_STYLE_COLOUR('',#11975);
#11977=FILL_AREA_STYLE('',(#11976));
#11978=SURFACE_STYLE_FILL_AREA(#11977);
#11979=SURFACE_SIDE_STYLE('',(#11978));
#11980=SURFACE_STYLE_USAGE(.BOTH.,#11979);
#11981=PRESENTATION_STYLE_ASSIGNMENT((#11980));
ENDSEC;
END-ISO-10303-21;
